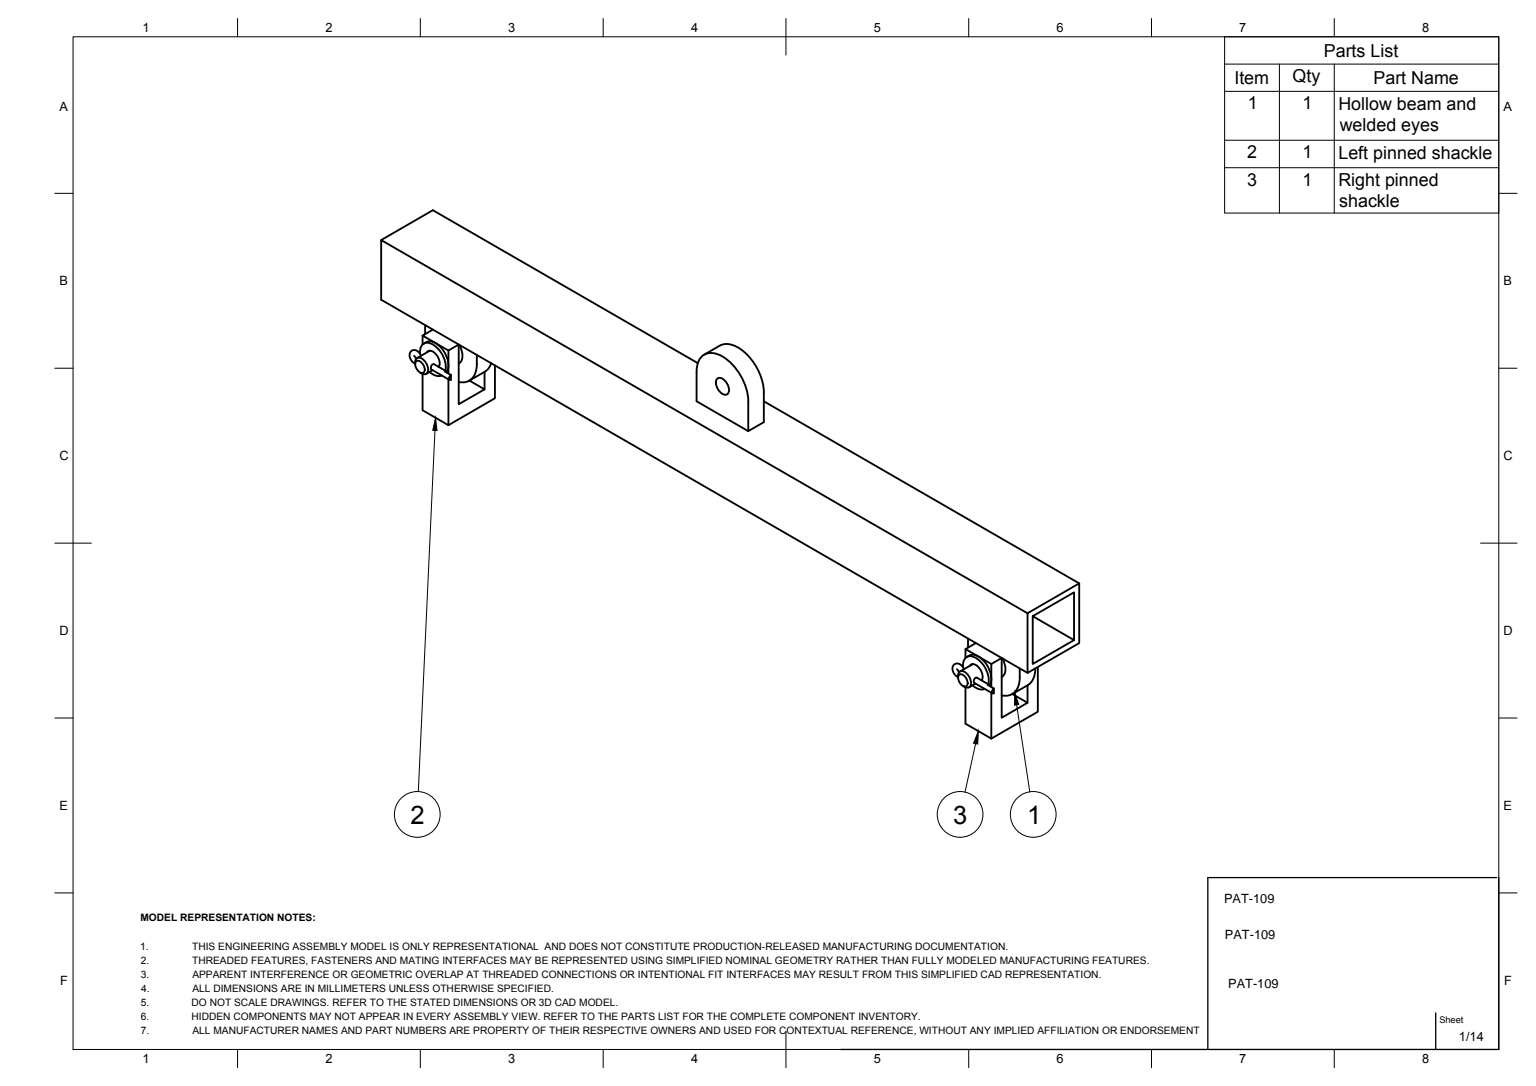
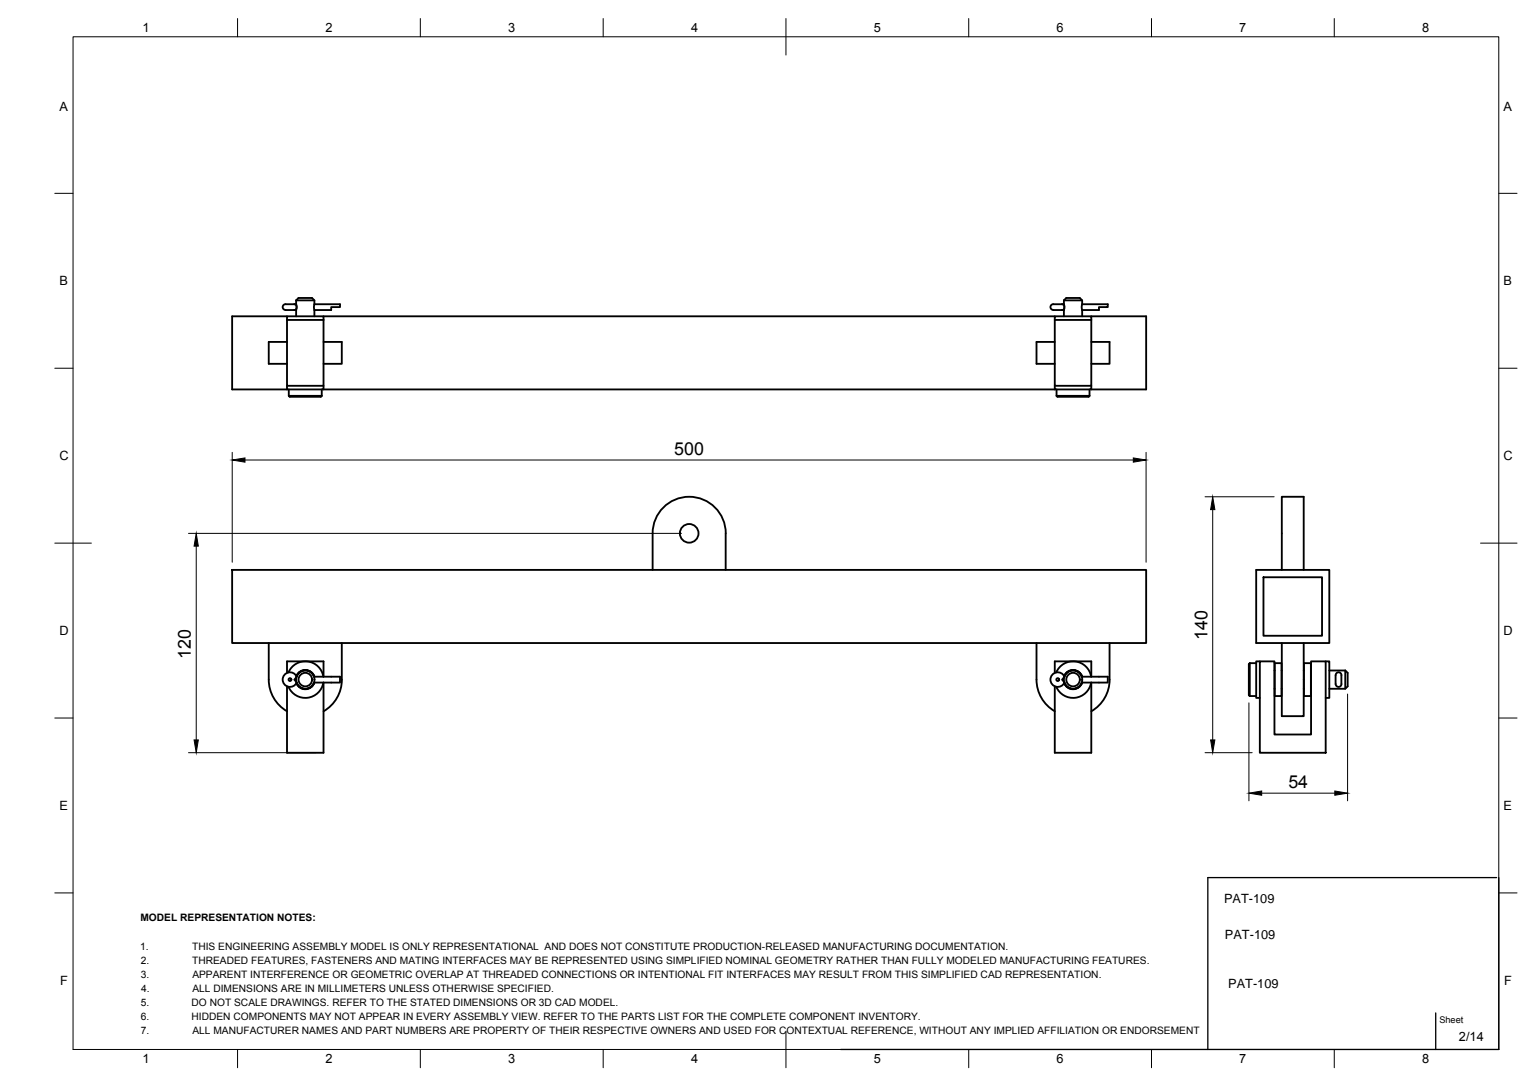
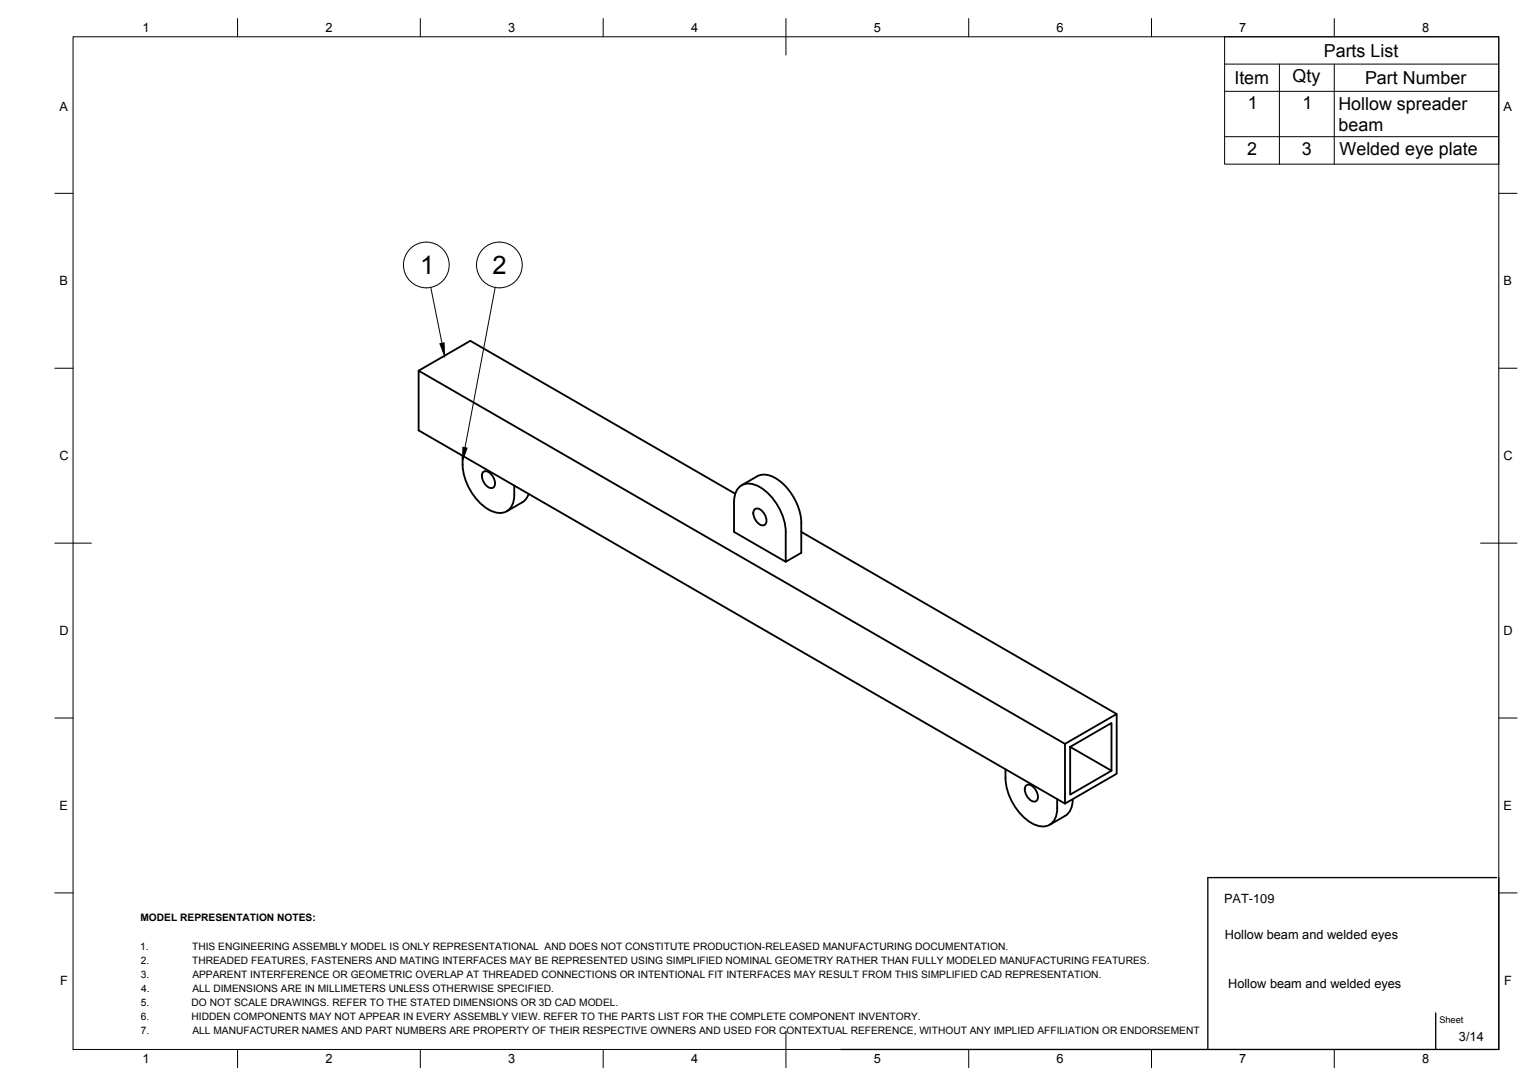
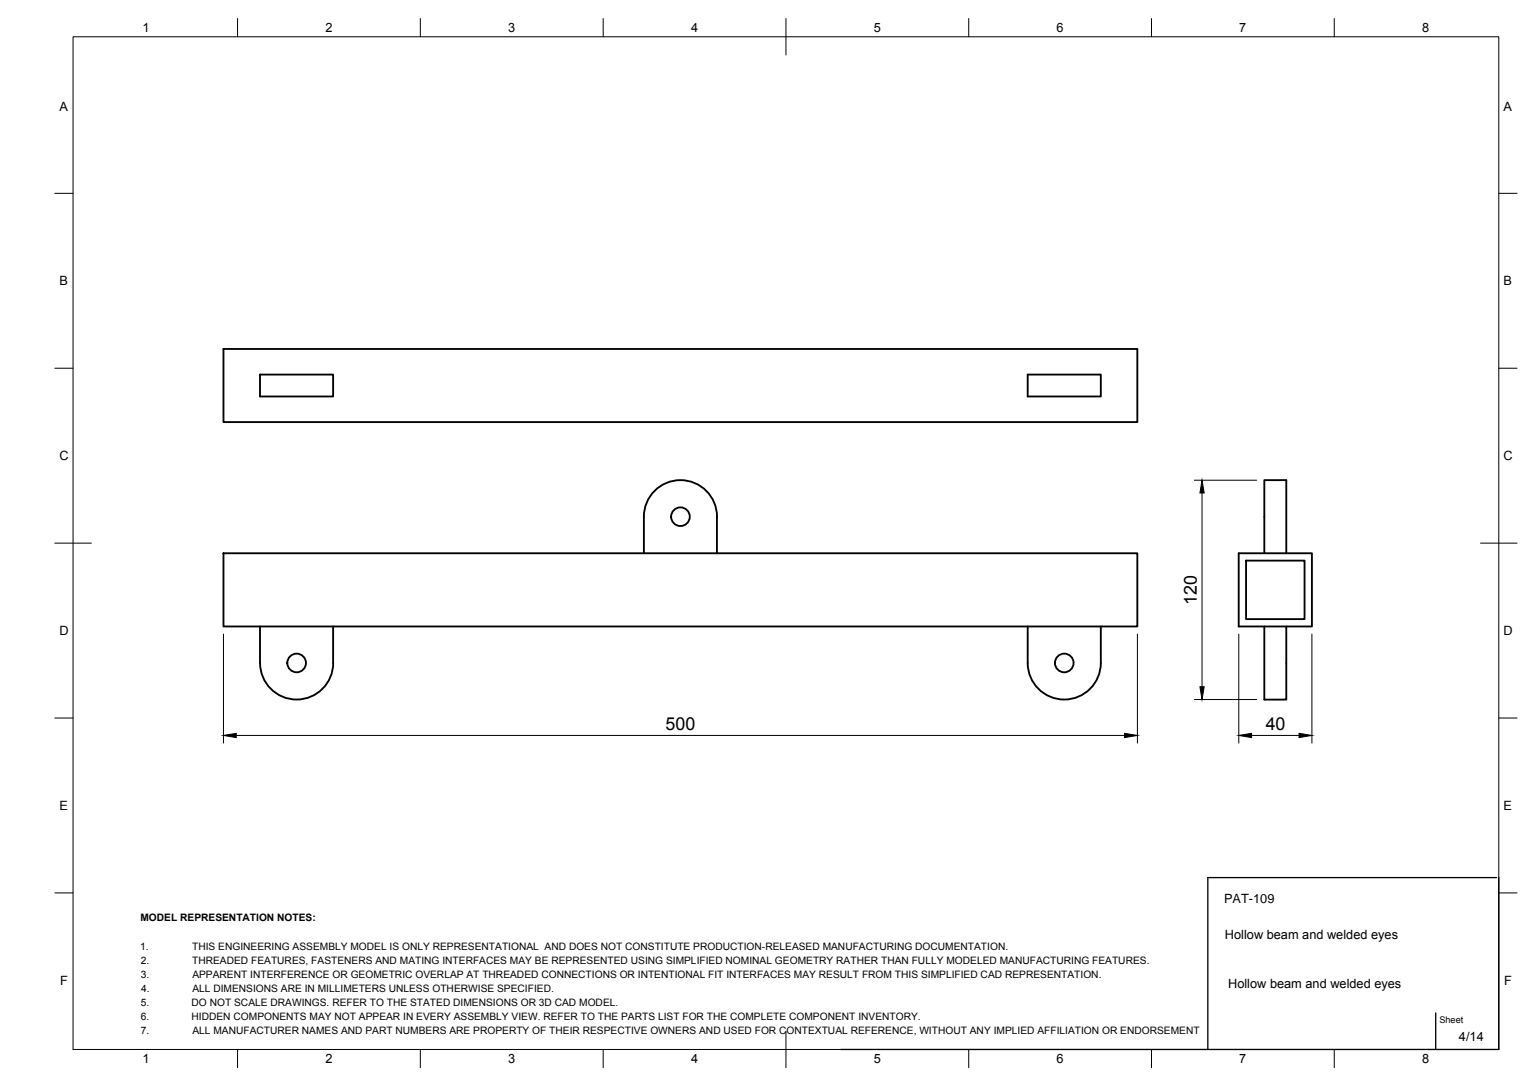
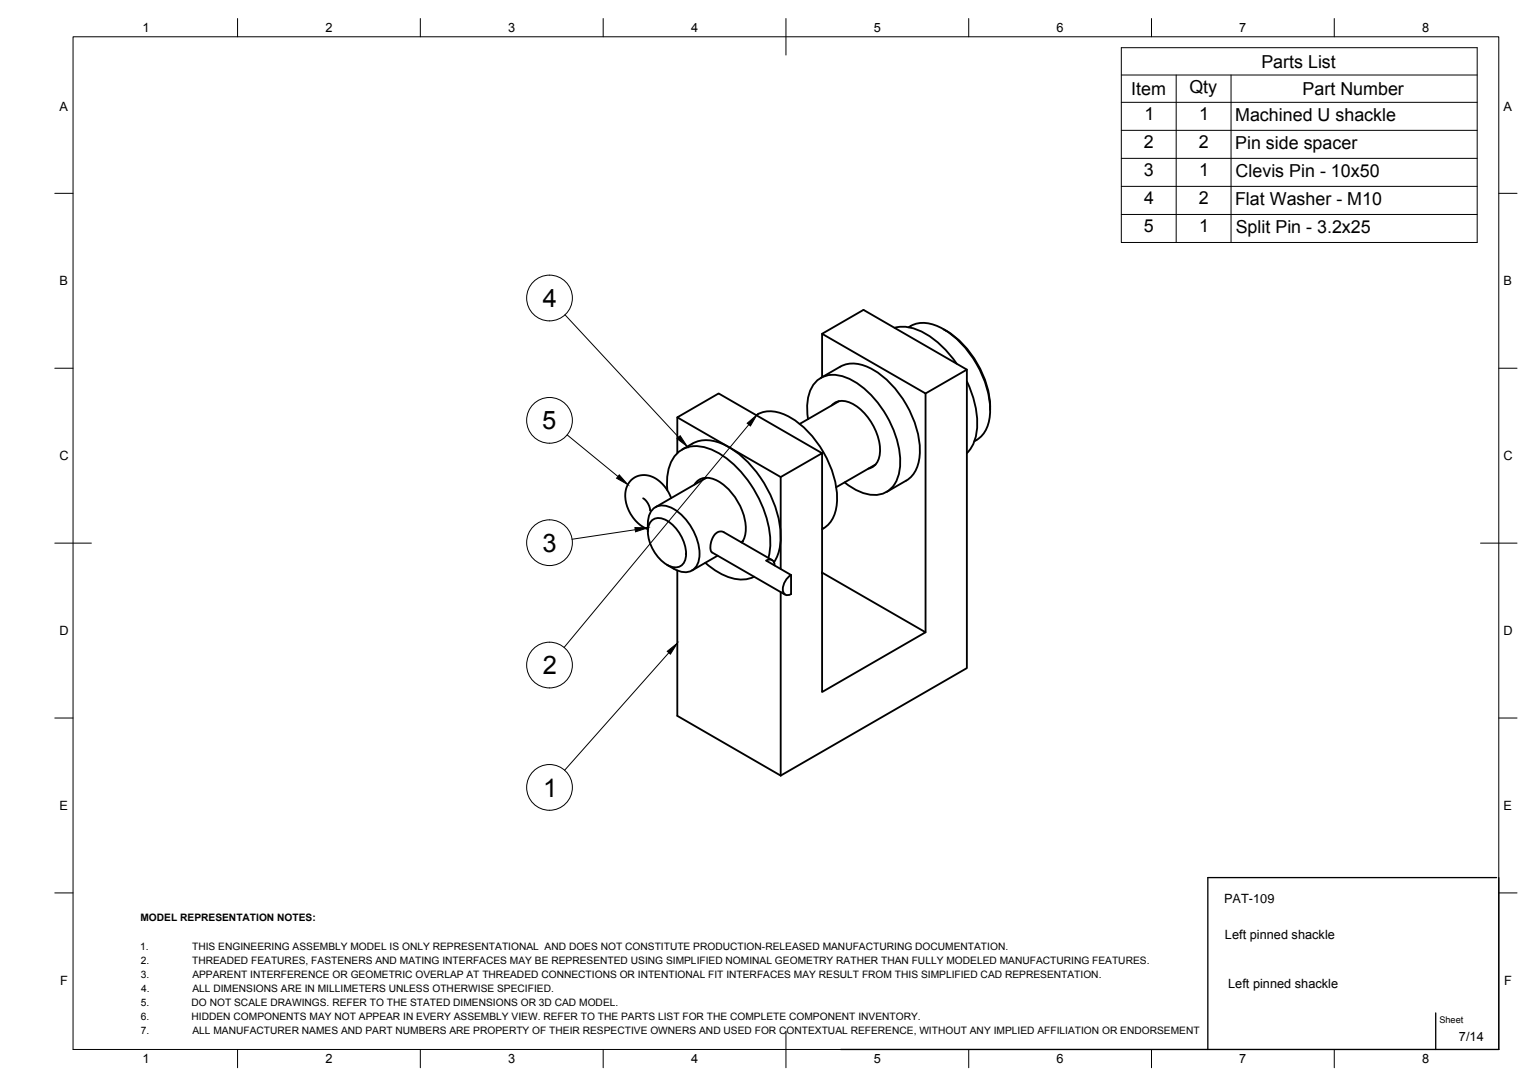
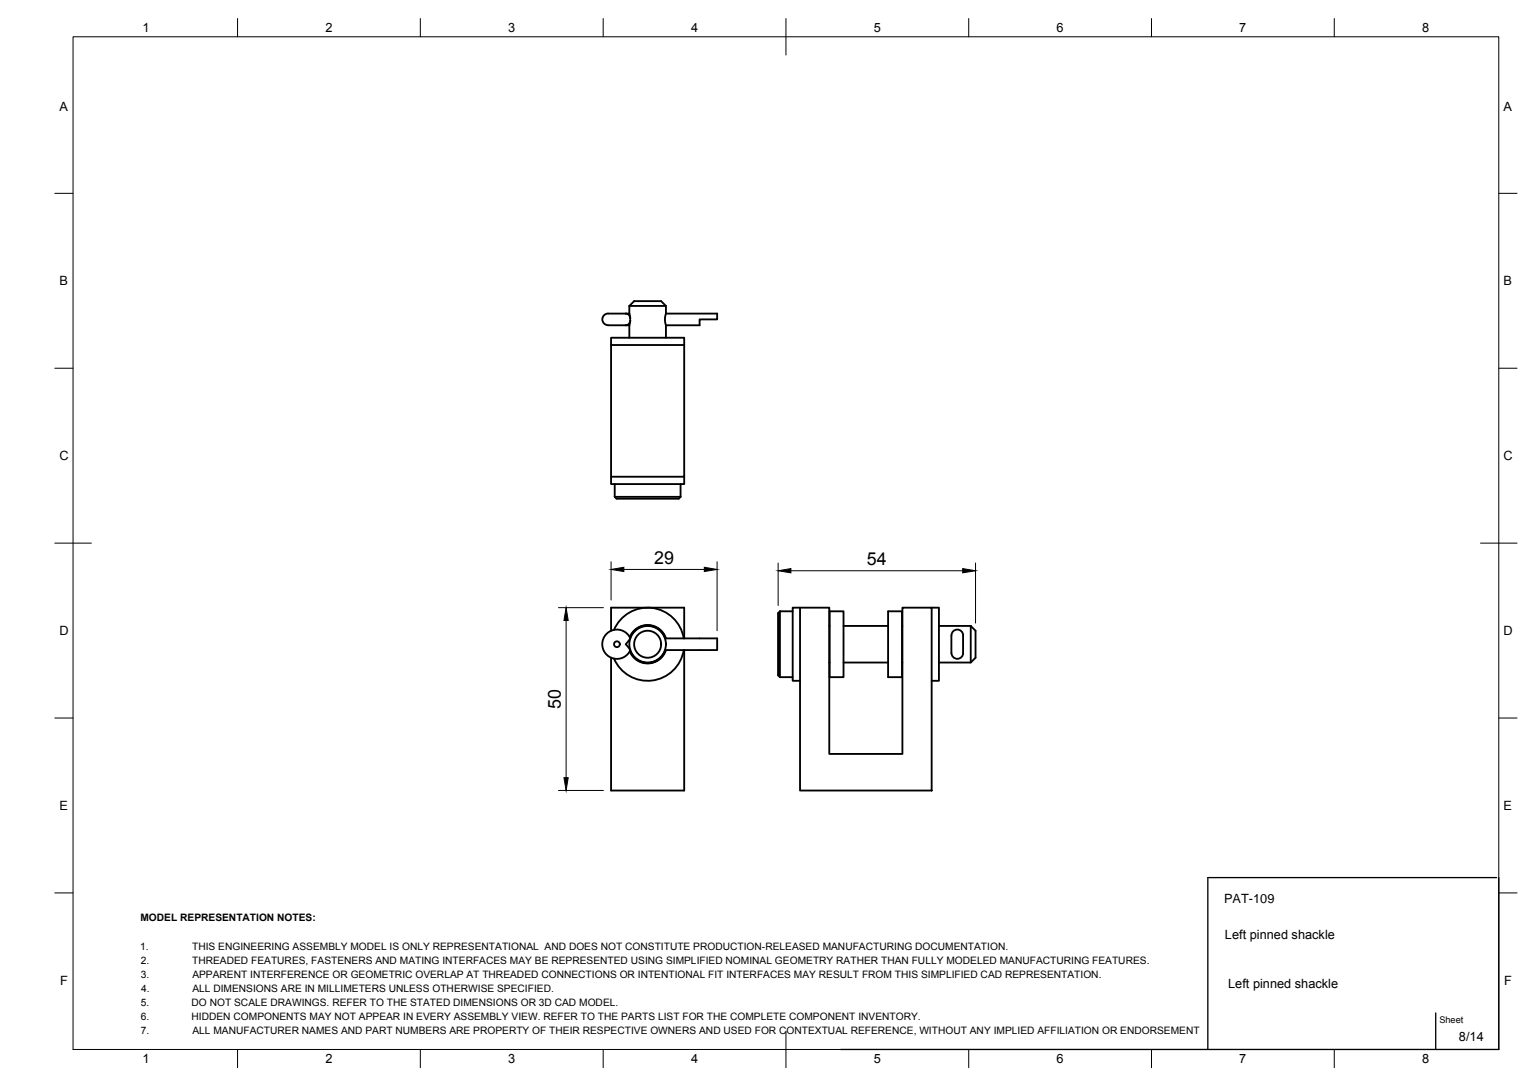
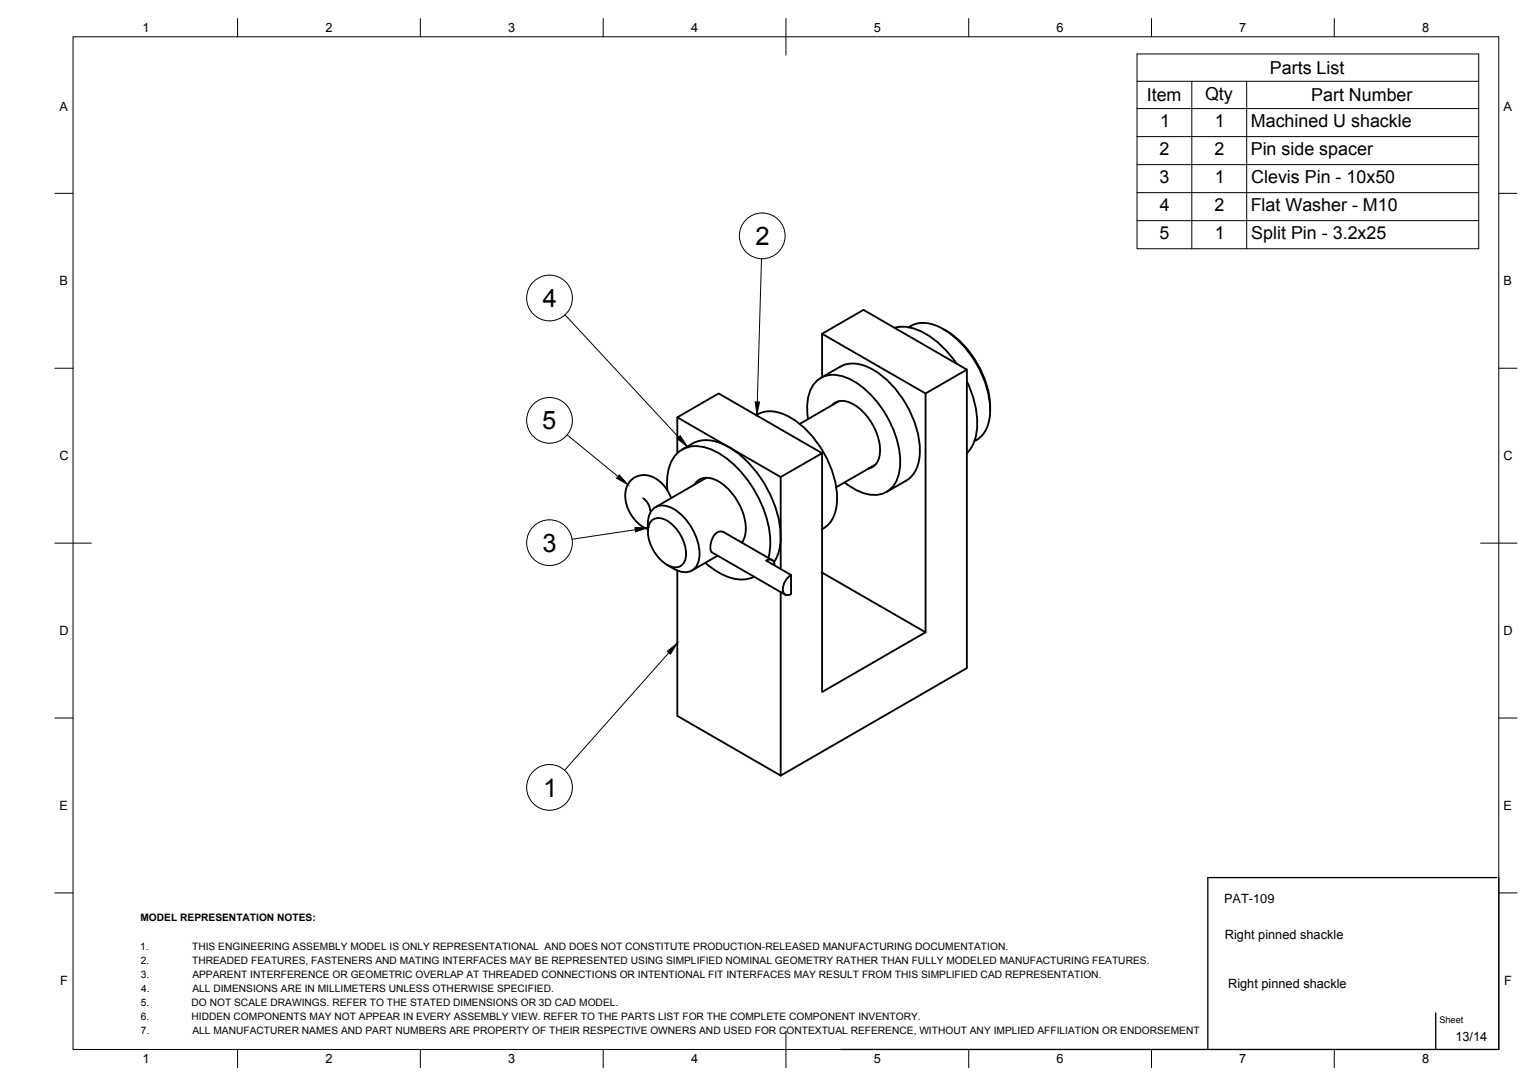
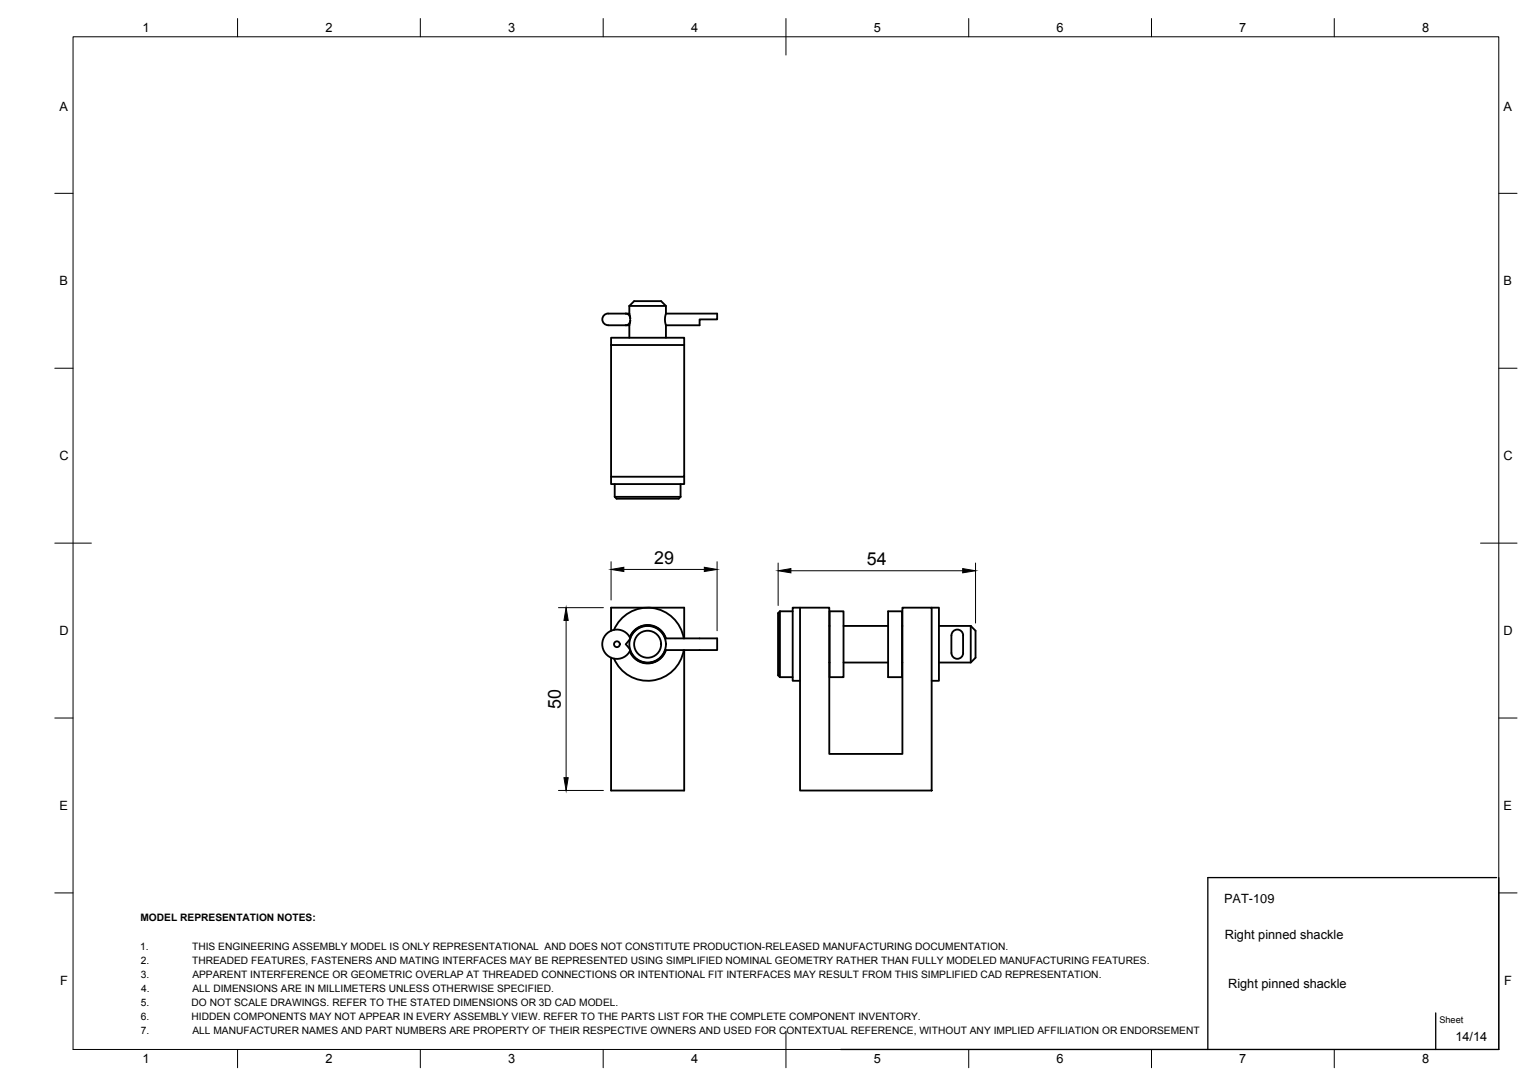
ISO-10303-21;
HEADER;
/* Generated by software containing ST-Developer
 * from STEP Tools, Inc. (www.steptools.com) 
 */

FILE_DESCRIPTION(
/* description */ ('Twin-shackle spreader bar'),
/* implementation_level */ '2;1');

FILE_NAME(
/* name */ 'PAT-109',
/* time_stamp */ '2026-10-27T20:18:10-07:00',
/* author */ (''),
/* organization */ (''),
/* preprocessor_version */ 'ST-DEVELOPER v20.2',
/* originating_system */ 'Autodesk Translation Framework v15.17.0.0',
/* authorisation */ '');

FILE_SCHEMA (('AUTOMOTIVE_DESIGN { 1 0 10303 214 3 1 1 }'));
ENDSEC;

DATA;
#10=MECHANICAL_DESIGN_GEOMETRIC_PRESENTATION_REPRESENTATION('',(#157,#158,
#159,#160,#161,#162,#163),#1829);
#11=TOROIDAL_SURFACE('',#1104,0.24,0.16);
#12=CONICAL_SURFACE('',#1083,0.875,0.785398163397448);
#13=CONICAL_SURFACE('',#1091,0.435,0.785398163397449);
#14=B_SPLINE_CURVE_WITH_KNOTS('',3,(#1599,#1600,#1601,#1602,#1603,#1604,
#1605,#1606,#1607,#1608),.UNSPECIFIED.,.F.,.F.,(4,2,2,2,4),(0.,0.0607460470679908,
0.121492094135982,0.182214421454286,0.242936748772591),.UNSPECIFIED.);
#15=B_SPLINE_CURVE_WITH_KNOTS('',3,(#1611,#1612,#1613,#1614,#1615,#1616,
#1617,#1618,#1619,#1620,#1621,#1622,#1623,#1624,#1625,#1626,#1627,#1628,
#1629,#1630,#1631,#1632,#1633,#1634,#1635,#1636,#1637,#1638,#1639,#1640,
#1641,#1642,#1643,#1644),.UNSPECIFIED.,.T.,.F.,(4,2,2,2,2,2,2,2,2,2,2,2,
2,2,2,2,4),(0.,0.0607460470679913,0.121492094135983,0.182214421454287,0.242936748772591,
0.303659076090896,0.3643814034092,0.425127450477191,0.485873497545182,0.546619544613173,
0.607365591681164,0.668087918999469,0.728810246317773,0.789532573636077,
0.850254900954382,0.911000948022373,0.971746995090363),.UNSPECIFIED.);
#16=B_SPLINE_CURVE_WITH_KNOTS('',3,(#1646,#1647,#1648,#1649,#1650,#1651,
#1652,#1653,#1654,#1655),.UNSPECIFIED.,.F.,.F.,(4,2,2,2,4),(0.728810246317772,
0.789532573636077,0.850254900954381,0.911000948022372,0.971746995090363),
 .UNSPECIFIED.);
#17=B_SPLINE_CURVE_WITH_KNOTS('',3,(#1656,#1657,#1658,#1659,#1660,#1661,
#1662,#1663,#1664,#1665,#1666,#1667,#1668,#1669,#1670,#1671,#1672,#1673),
 .UNSPECIFIED.,.F.,.F.,(4,2,2,2,2,2,2,2,4),(0.242936748772591,0.303659076090895,
0.364381403409199,0.42512745047719,0.485873497545182,0.546619544613173,
0.607365591681163,0.668087918999468,0.728810246317772),.UNSPECIFIED.);
#18=B_SPLINE_CURVE_WITH_KNOTS('',3,(#1720,#1721,#1722,#1723,#1724,#1725,
#1726,#1727,#1728,#1729,#1730,#1731,#1732,#1733,#1734,#1735,#1736,#1737,
#1738,#1739,#1740,#1741,#1742,#1743,#1744,#1745),.UNSPECIFIED.,.F.,.F.,
(4,2,2,2,2,2,2,2,2,2,2,2,4),(-0.000771405883143509,0.,0.0566386712389912,
0.124022719697233,0.181497823731714,0.241714216509916,0.290259365558526,
0.338804514607135,0.399020907385337,0.456496011419817,0.52388005987806,
0.580518731117043,0.581290137000192),.UNSPECIFIED.);
#19=B_SPLINE_CURVE_WITH_KNOTS('',3,(#1746,#1747,#1748,#1749,#1750,#1751,
#1752,#1753,#1754,#1755,#1756,#1757,#1758,#1759,#1760,#1761,#1762,#1763,
#1764,#1765,#1766,#1767,#1768,#1769,#1770,#1771),.UNSPECIFIED.,.F.,.F.,
(4,2,2,2,2,2,2,2,2,2,2,2,4),(-0.000771405883162359,0.,0.0566386712397236,
0.124022719698972,0.181497823734311,0.241714216513412,0.290259365562747,
0.338804514612082,0.399020907391184,0.456496011426523,0.523880059885771,
0.580518731125564,0.58129013700872),.UNSPECIFIED.);
#20=ITEM_DEFINED_TRANSFORMATION($,$,#1024,#1047);
#21=ITEM_DEFINED_TRANSFORMATION($,$,#1035,#1048);
#22=ITEM_DEFINED_TRANSFORMATION($,$,#1035,#1049);
#23=ITEM_DEFINED_TRANSFORMATION($,$,#1035,#1050);
#24=ITEM_DEFINED_TRANSFORMATION($,$,#1053,#1114);
#25=ITEM_DEFINED_TRANSFORMATION($,$,#1070,#1115);
#26=ITEM_DEFINED_TRANSFORMATION($,$,#1070,#1116);
#27=ITEM_DEFINED_TRANSFORMATION($,$,#1079,#1117);
#28=ITEM_DEFINED_TRANSFORMATION($,$,#1094,#1118);
#29=ITEM_DEFINED_TRANSFORMATION($,$,#1094,#1119);
#30=ITEM_DEFINED_TRANSFORMATION($,$,#1103,#1120);
#31=ITEM_DEFINED_TRANSFORMATION($,$,#1053,#1121);
#32=ITEM_DEFINED_TRANSFORMATION($,$,#1070,#1122);
#33=ITEM_DEFINED_TRANSFORMATION($,$,#1070,#1123);
#34=ITEM_DEFINED_TRANSFORMATION($,$,#1079,#1124);
#35=ITEM_DEFINED_TRANSFORMATION($,$,#1094,#1125);
#36=ITEM_DEFINED_TRANSFORMATION($,$,#1094,#1126);
#37=ITEM_DEFINED_TRANSFORMATION($,$,#1103,#1127);
#38=ITEM_DEFINED_TRANSFORMATION($,$,#1023,#1128);
#39=ITEM_DEFINED_TRANSFORMATION($,$,#1051,#1129);
#40=ITEM_DEFINED_TRANSFORMATION($,$,#1052,#1130);
#41=(
REPRESENTATION_RELATIONSHIP($,$,#1879,#1878)
REPRESENTATION_RELATIONSHIP_WITH_TRANSFORMATION(#20)
SHAPE_REPRESENTATION_RELATIONSHIP()
);
#42=(
REPRESENTATION_RELATIONSHIP($,$,#1880,#1878)
REPRESENTATION_RELATIONSHIP_WITH_TRANSFORMATION(#21)
SHAPE_REPRESENTATION_RELATIONSHIP()
);
#43=(
REPRESENTATION_RELATIONSHIP($,$,#1880,#1878)
REPRESENTATION_RELATIONSHIP_WITH_TRANSFORMATION(#22)
SHAPE_REPRESENTATION_RELATIONSHIP()
);
#44=(
REPRESENTATION_RELATIONSHIP($,$,#1880,#1878)
REPRESENTATION_RELATIONSHIP_WITH_TRANSFORMATION(#23)
SHAPE_REPRESENTATION_RELATIONSHIP()
);
#45=(
REPRESENTATION_RELATIONSHIP($,$,#1883,#1881)
REPRESENTATION_RELATIONSHIP_WITH_TRANSFORMATION(#24)
SHAPE_REPRESENTATION_RELATIONSHIP()
);
#46=(
REPRESENTATION_RELATIONSHIP($,$,#1884,#1881)
REPRESENTATION_RELATIONSHIP_WITH_TRANSFORMATION(#25)
SHAPE_REPRESENTATION_RELATIONSHIP()
);
#47=(
REPRESENTATION_RELATIONSHIP($,$,#1884,#1881)
REPRESENTATION_RELATIONSHIP_WITH_TRANSFORMATION(#26)
SHAPE_REPRESENTATION_RELATIONSHIP()
);
#48=(
REPRESENTATION_RELATIONSHIP($,$,#1885,#1881)
REPRESENTATION_RELATIONSHIP_WITH_TRANSFORMATION(#27)
SHAPE_REPRESENTATION_RELATIONSHIP()
);
#49=(
REPRESENTATION_RELATIONSHIP($,$,#1886,#1881)
REPRESENTATION_RELATIONSHIP_WITH_TRANSFORMATION(#28)
SHAPE_REPRESENTATION_RELATIONSHIP()
);
#50=(
REPRESENTATION_RELATIONSHIP($,$,#1886,#1881)
REPRESENTATION_RELATIONSHIP_WITH_TRANSFORMATION(#29)
SHAPE_REPRESENTATION_RELATIONSHIP()
);
#51=(
REPRESENTATION_RELATIONSHIP($,$,#1887,#1881)
REPRESENTATION_RELATIONSHIP_WITH_TRANSFORMATION(#30)
SHAPE_REPRESENTATION_RELATIONSHIP()
);
#52=(
REPRESENTATION_RELATIONSHIP($,$,#1883,#1882)
REPRESENTATION_RELATIONSHIP_WITH_TRANSFORMATION(#31)
SHAPE_REPRESENTATION_RELATIONSHIP()
);
#53=(
REPRESENTATION_RELATIONSHIP($,$,#1884,#1882)
REPRESENTATION_RELATIONSHIP_WITH_TRANSFORMATION(#32)
SHAPE_REPRESENTATION_RELATIONSHIP()
);
#54=(
REPRESENTATION_RELATIONSHIP($,$,#1884,#1882)
REPRESENTATION_RELATIONSHIP_WITH_TRANSFORMATION(#33)
SHAPE_REPRESENTATION_RELATIONSHIP()
);
#55=(
REPRESENTATION_RELATIONSHIP($,$,#1885,#1882)
REPRESENTATION_RELATIONSHIP_WITH_TRANSFORMATION(#34)
SHAPE_REPRESENTATION_RELATIONSHIP()
);
#56=(
REPRESENTATION_RELATIONSHIP($,$,#1886,#1882)
REPRESENTATION_RELATIONSHIP_WITH_TRANSFORMATION(#35)
SHAPE_REPRESENTATION_RELATIONSHIP()
);
#57=(
REPRESENTATION_RELATIONSHIP($,$,#1886,#1882)
REPRESENTATION_RELATIONSHIP_WITH_TRANSFORMATION(#36)
SHAPE_REPRESENTATION_RELATIONSHIP()
);
#58=(
REPRESENTATION_RELATIONSHIP($,$,#1887,#1882)
REPRESENTATION_RELATIONSHIP_WITH_TRANSFORMATION(#37)
SHAPE_REPRESENTATION_RELATIONSHIP()
);
#59=(
REPRESENTATION_RELATIONSHIP($,$,#1878,#1877)
REPRESENTATION_RELATIONSHIP_WITH_TRANSFORMATION(#38)
SHAPE_REPRESENTATION_RELATIONSHIP()
);
#60=(
REPRESENTATION_RELATIONSHIP($,$,#1881,#1877)
REPRESENTATION_RELATIONSHIP_WITH_TRANSFORMATION(#39)
SHAPE_REPRESENTATION_RELATIONSHIP()
);
#61=(
REPRESENTATION_RELATIONSHIP($,$,#1882,#1877)
REPRESENTATION_RELATIONSHIP_WITH_TRANSFORMATION(#40)
SHAPE_REPRESENTATION_RELATIONSHIP()
);
#62=CONTEXT_DEPENDENT_SHAPE_REPRESENTATION(#41,#1849);
#63=CONTEXT_DEPENDENT_SHAPE_REPRESENTATION(#42,#1850);
#64=CONTEXT_DEPENDENT_SHAPE_REPRESENTATION(#43,#1851);
#65=CONTEXT_DEPENDENT_SHAPE_REPRESENTATION(#44,#1852);
#66=CONTEXT_DEPENDENT_SHAPE_REPRESENTATION(#45,#1860);
#67=CONTEXT_DEPENDENT_SHAPE_REPRESENTATION(#46,#1861);
#68=CONTEXT_DEPENDENT_SHAPE_REPRESENTATION(#47,#1862);
#69=CONTEXT_DEPENDENT_SHAPE_REPRESENTATION(#48,#1863);
#70=CONTEXT_DEPENDENT_SHAPE_REPRESENTATION(#49,#1864);
#71=CONTEXT_DEPENDENT_SHAPE_REPRESENTATION(#50,#1865);
#72=CONTEXT_DEPENDENT_SHAPE_REPRESENTATION(#51,#1866);
#73=CONTEXT_DEPENDENT_SHAPE_REPRESENTATION(#52,#1867);
#74=CONTEXT_DEPENDENT_SHAPE_REPRESENTATION(#53,#1868);
#75=CONTEXT_DEPENDENT_SHAPE_REPRESENTATION(#54,#1869);
#76=CONTEXT_DEPENDENT_SHAPE_REPRESENTATION(#55,#1870);
#77=CONTEXT_DEPENDENT_SHAPE_REPRESENTATION(#56,#1871);
#78=CONTEXT_DEPENDENT_SHAPE_REPRESENTATION(#57,#1872);
#79=CONTEXT_DEPENDENT_SHAPE_REPRESENTATION(#58,#1873);
#80=CONTEXT_DEPENDENT_SHAPE_REPRESENTATION(#59,#1874);
#81=CONTEXT_DEPENDENT_SHAPE_REPRESENTATION(#60,#1875);
#82=CONTEXT_DEPENDENT_SHAPE_REPRESENTATION(#61,#1876);
#83=NEXT_ASSEMBLY_USAGE_OCCURRENCE('Hollow spreader beam:1',
'Hollow spreader beam:1','Hollow spreader beam:1',#1890,#1891,
'Hollow spreader beam:1');
#84=NEXT_ASSEMBLY_USAGE_OCCURRENCE('Welded eye plate:1',
'Welded eye plate:1','Welded eye plate:1',#1890,#1892,
'Welded eye plate:1');
#85=NEXT_ASSEMBLY_USAGE_OCCURRENCE('Welded eye plate:2',
'Welded eye plate:2','Welded eye plate:2',#1890,#1892,
'Welded eye plate:2');
#86=NEXT_ASSEMBLY_USAGE_OCCURRENCE('Welded eye plate:3',
'Welded eye plate:3','Welded eye plate:3',#1890,#1892,
'Welded eye plate:3');
#87=NEXT_ASSEMBLY_USAGE_OCCURRENCE('Machined U shackle:1',
'Machined U shackle:1','Machined U shackle:1',#1893,#1895,
'Machined U shackle:1');
#88=NEXT_ASSEMBLY_USAGE_OCCURRENCE('Pin side spacer:1',
'Pin side spacer:1','Pin side spacer:1',#1893,#1896,'Pin side spacer:1');
#89=NEXT_ASSEMBLY_USAGE_OCCURRENCE('Pin side spacer:2',
'Pin side spacer:2','Pin side spacer:2',#1893,#1896,'Pin side spacer:2');
#90=NEXT_ASSEMBLY_USAGE_OCCURRENCE('Clevis Pin - 10x50:2',
'Clevis Pin - 10x50:2','Clevis Pin - 10x50:2',#1893,#1897,
'Clevis Pin - 10x50:2');
#91=NEXT_ASSEMBLY_USAGE_OCCURRENCE('Flat Washer - M10:2',
'Flat Washer - M10:2','Flat Washer - M10:2',#1893,#1898,
'Flat Washer - M10:2');
#92=NEXT_ASSEMBLY_USAGE_OCCURRENCE('Flat Washer - M10:3',
'Flat Washer - M10:3','Flat Washer - M10:3',#1893,#1898,
'Flat Washer - M10:3');
#93=NEXT_ASSEMBLY_USAGE_OCCURRENCE('Split Pin - 3.2x25:2',
'Split Pin - 3.2x25:2','Split Pin - 3.2x25:2',#1893,#1899,
'Split Pin - 3.2x25:2');
#94=NEXT_ASSEMBLY_USAGE_OCCURRENCE('Machined U shackle:2',
'Machined U shackle:2','Machined U shackle:2',#1894,#1895,
'Machined U shackle:2');
#95=NEXT_ASSEMBLY_USAGE_OCCURRENCE('Pin side spacer:3',
'Pin side spacer:3','Pin side spacer:3',#1894,#1896,'Pin side spacer:3');
#96=NEXT_ASSEMBLY_USAGE_OCCURRENCE('Pin side spacer:4',
'Pin side spacer:4','Pin side spacer:4',#1894,#1896,'Pin side spacer:4');
#97=NEXT_ASSEMBLY_USAGE_OCCURRENCE('Clevis Pin - 10x50:3',
'Clevis Pin - 10x50:3','Clevis Pin - 10x50:3',#1894,#1897,
'Clevis Pin - 10x50:3');
#98=NEXT_ASSEMBLY_USAGE_OCCURRENCE('Flat Washer - M10:4',
'Flat Washer - M10:4','Flat Washer - M10:4',#1894,#1898,
'Flat Washer - M10:4');
#99=NEXT_ASSEMBLY_USAGE_OCCURRENCE('Flat Washer - M10:5',
'Flat Washer - M10:5','Flat Washer - M10:5',#1894,#1898,
'Flat Washer - M10:5');
#100=NEXT_ASSEMBLY_USAGE_OCCURRENCE('Split Pin - 3.2x25:3',
'Split Pin - 3.2x25:3','Split Pin - 3.2x25:3',#1894,#1899,
'Split Pin - 3.2x25:3');
#101=NEXT_ASSEMBLY_USAGE_OCCURRENCE('Hollow beam and welded eyes:1',
'Hollow beam and welded eyes:1','Hollow beam and welded eyes:1',#1889,#1890,
'Hollow beam and welded eyes:1');
#102=NEXT_ASSEMBLY_USAGE_OCCURRENCE('Left pinned shackle:1',
'Left pinned shackle:1','Left pinned shackle:1',#1889,#1893,
'Left pinned shackle:1');
#103=NEXT_ASSEMBLY_USAGE_OCCURRENCE('Right pinned shackle:1',
'Right pinned shackle:1','Right pinned shackle:1',#1889,#1894,
'Right pinned shackle:1');
#104=CIRCLE('',#1037,0.510000000000002);
#105=CIRCLE('',#1038,0.510000000000002);
#106=CIRCLE('',#1043,2.);
#107=CIRCLE('',#1045,2.);
#108=CIRCLE('',#1055,0.515000000000001);
#109=CIRCLE('',#1056,0.515000000000001);
#110=CIRCLE('',#1058,0.515000000000001);
#111=CIRCLE('',#1059,0.515000000000001);
#112=CIRCLE('',#1072,0.510000000000002);
#113=CIRCLE('',#1073,0.510000000000002);
#114=CIRCLE('',#1075,0.899999999999999);
#115=CIRCLE('',#1076,0.899999999999999);
#116=CIRCLE('',#1082,0.85);
#117=CIRCLE('',#1084,0.9);
#118=CIRCLE('',#1086,0.9);
#119=CIRCLE('',#1088,0.5);
#120=CIRCLE('',#1090,0.5);
#121=CIRCLE('',#1092,0.37);
#122=CIRCLE('',#1096,0.525);
#123=CIRCLE('',#1097,0.525);
#124=CIRCLE('',#1099,1.);
#125=CIRCLE('',#1100,1.);
#126=CIRCLE('',#1105,0.16);
#127=CIRCLE('',#1106,0.08);
#128=CIRCLE('',#1108,0.16);
#129=CIRCLE('',#1111,0.16);
#130=CIRCLE('',#1112,0.16);
#131=CYLINDRICAL_SURFACE('',#1036,0.510000000000002);
#132=CYLINDRICAL_SURFACE('',#1044,2.);
#133=CYLINDRICAL_SURFACE('',#1054,0.515000000000001);
#134=CYLINDRICAL_SURFACE('',#1057,0.515000000000001);
#135=CYLINDRICAL_SURFACE('',#1071,0.510000000000002);
#136=CYLINDRICAL_SURFACE('',#1074,0.899999999999999);
#137=CYLINDRICAL_SURFACE('',#1080,0.16);
#138=CYLINDRICAL_SURFACE('',#1085,0.9);
#139=CYLINDRICAL_SURFACE('',#1089,0.5);
#140=CYLINDRICAL_SURFACE('',#1095,0.525);
#141=CYLINDRICAL_SURFACE('',#1098,1.);
#142=CYLINDRICAL_SURFACE('',#1110,0.16);
#143=SHAPE_REPRESENTATION_RELATIONSHIP('SRR','None',#1879,#150);
#144=SHAPE_REPRESENTATION_RELATIONSHIP('SRR','None',#1880,#151);
#145=SHAPE_REPRESENTATION_RELATIONSHIP('SRR','None',#1883,#152);
#146=SHAPE_REPRESENTATION_RELATIONSHIP('SRR','None',#1884,#153);
#147=SHAPE_REPRESENTATION_RELATIONSHIP('SRR','None',#1885,#154);
#148=SHAPE_REPRESENTATION_RELATIONSHIP('SRR','None',#1886,#155);
#149=SHAPE_REPRESENTATION_RELATIONSHIP('SRR','None',#1887,#156);
#150=ADVANCED_BREP_SHAPE_REPRESENTATION('',(#164),#1820);
#151=ADVANCED_BREP_SHAPE_REPRESENTATION('',(#165),#1821);
#152=ADVANCED_BREP_SHAPE_REPRESENTATION('',(#166),#1824);
#153=ADVANCED_BREP_SHAPE_REPRESENTATION('',(#167),#1825);
#154=ADVANCED_BREP_SHAPE_REPRESENTATION('',(#168),#1826);
#155=ADVANCED_BREP_SHAPE_REPRESENTATION('',(#169),#1827);
#156=ADVANCED_BREP_SHAPE_REPRESENTATION('',(#170),#1828);
#157=STYLED_ITEM('',(#1977),#164);
#158=STYLED_ITEM('',(#1977),#165);
#159=STYLED_ITEM('',(#1970),#166);
#160=STYLED_ITEM('',(#1984),#167);
#161=STYLED_ITEM('',(#1984),#168);
#162=STYLED_ITEM('',(#1991),#169);
#163=STYLED_ITEM('',(#1984),#170);
#164=MANIFOLD_SOLID_BREP('Body1',#937);
#165=MANIFOLD_SOLID_BREP('Body1',#938);
#166=MANIFOLD_SOLID_BREP('Body1',#939);
#167=MANIFOLD_SOLID_BREP('Body1',#940);
#168=MANIFOLD_SOLID_BREP('Body1',#941);
#169=MANIFOLD_SOLID_BREP('Body1',#942);
#170=MANIFOLD_SOLID_BREP('Body1',#943);
#171=FACE_BOUND('',#242,.T.);
#172=FACE_BOUND('',#245,.T.);
#173=FACE_BOUND('',#253,.T.);
#174=FACE_BOUND('',#256,.T.);
#175=FACE_BOUND('',#260,.T.);
#176=FACE_BOUND('',#263,.T.);
#177=FACE_BOUND('',#266,.T.);
#178=FACE_BOUND('',#269,.T.);
#179=FACE_BOUND('',#276,.T.);
#180=FACE_BOUND('',#278,.T.);
#181=FACE_BOUND('',#284,.T.);
#182=FACE_BOUND('',#286,.T.);
#183=FACE_BOUND('',#292,.T.);
#184=FACE_BOUND('',#294,.T.);
#185=FACE_BOUND('',#296,.T.);
#186=FACE_OUTER_BOUND('',#236,.T.);
#187=FACE_OUTER_BOUND('',#237,.T.);
#188=FACE_OUTER_BOUND('',#238,.T.);
#189=FACE_OUTER_BOUND('',#239,.T.);
#190=FACE_OUTER_BOUND('',#240,.T.);
#191=FACE_OUTER_BOUND('',#241,.T.);
#192=FACE_OUTER_BOUND('',#243,.T.);
#193=FACE_OUTER_BOUND('',#244,.T.);
#194=FACE_OUTER_BOUND('',#246,.T.);
#195=FACE_OUTER_BOUND('',#247,.T.);
#196=FACE_OUTER_BOUND('',#248,.T.);
#197=FACE_OUTER_BOUND('',#249,.T.);
#198=FACE_OUTER_BOUND('',#250,.T.);
#199=FACE_OUTER_BOUND('',#251,.T.);
#200=FACE_OUTER_BOUND('',#252,.T.);
#201=FACE_OUTER_BOUND('',#254,.T.);
#202=FACE_OUTER_BOUND('',#255,.T.);
#203=FACE_OUTER_BOUND('',#257,.T.);
#204=FACE_OUTER_BOUND('',#258,.T.);
#205=FACE_OUTER_BOUND('',#259,.T.);
#206=FACE_OUTER_BOUND('',#261,.T.);
#207=FACE_OUTER_BOUND('',#262,.T.);
#208=FACE_OUTER_BOUND('',#264,.T.);
#209=FACE_OUTER_BOUND('',#265,.T.);
#210=FACE_OUTER_BOUND('',#267,.T.);
#211=FACE_OUTER_BOUND('',#268,.T.);
#212=FACE_OUTER_BOUND('',#270,.T.);
#213=FACE_OUTER_BOUND('',#271,.T.);
#214=FACE_OUTER_BOUND('',#272,.T.);
#215=FACE_OUTER_BOUND('',#273,.T.);
#216=FACE_OUTER_BOUND('',#274,.T.);
#217=FACE_OUTER_BOUND('',#275,.T.);
#218=FACE_OUTER_BOUND('',#277,.T.);
#219=FACE_OUTER_BOUND('',#279,.T.);
#220=FACE_OUTER_BOUND('',#280,.T.);
#221=FACE_OUTER_BOUND('',#281,.T.);
#222=FACE_OUTER_BOUND('',#282,.T.);
#223=FACE_OUTER_BOUND('',#283,.T.);
#224=FACE_OUTER_BOUND('',#285,.T.);
#225=FACE_OUTER_BOUND('',#287,.T.);
#226=FACE_OUTER_BOUND('',#288,.T.);
#227=FACE_OUTER_BOUND('',#289,.T.);
#228=FACE_OUTER_BOUND('',#290,.T.);
#229=FACE_OUTER_BOUND('',#291,.T.);
#230=FACE_OUTER_BOUND('',#293,.T.);
#231=FACE_OUTER_BOUND('',#295,.T.);
#232=FACE_OUTER_BOUND('',#297,.T.);
#233=FACE_OUTER_BOUND('',#298,.T.);
#234=FACE_OUTER_BOUND('',#299,.T.);
#235=FACE_OUTER_BOUND('',#300,.T.);
#236=EDGE_LOOP('',(#634,#635,#636,#637));
#237=EDGE_LOOP('',(#638,#639,#640,#641));
#238=EDGE_LOOP('',(#642,#643,#644,#645));
#239=EDGE_LOOP('',(#646,#647,#648,#649));
#240=EDGE_LOOP('',(#650,#651,#652,#653));
#241=EDGE_LOOP('',(#654,#655,#656,#657));
#242=EDGE_LOOP('',(#658,#659,#660,#661));
#243=EDGE_LOOP('',(#662,#663,#664,#665));
#244=EDGE_LOOP('',(#666,#667,#668,#669));
#245=EDGE_LOOP('',(#670,#671,#672,#673));
#246=EDGE_LOOP('',(#674,#675,#676,#677));
#247=EDGE_LOOP('',(#678,#679,#680,#681));
#248=EDGE_LOOP('',(#682,#683,#684,#685));
#249=EDGE_LOOP('',(#686,#687,#688,#689));
#250=EDGE_LOOP('',(#690,#691,#692,#693));
#251=EDGE_LOOP('',(#694,#695,#696,#697));
#252=EDGE_LOOP('',(#698,#699,#700,#701));
#253=EDGE_LOOP('',(#702));
#254=EDGE_LOOP('',(#703,#704,#705,#706));
#255=EDGE_LOOP('',(#707,#708,#709,#710));
#256=EDGE_LOOP('',(#711));
#257=EDGE_LOOP('',(#712,#713,#714,#715));
#258=EDGE_LOOP('',(#716,#717,#718,#719));
#259=EDGE_LOOP('',(#720,#721,#722,#723));
#260=EDGE_LOOP('',(#724));
#261=EDGE_LOOP('',(#725,#726,#727,#728));
#262=EDGE_LOOP('',(#729,#730,#731,#732));
#263=EDGE_LOOP('',(#733));
#264=EDGE_LOOP('',(#734,#735,#736,#737));
#265=EDGE_LOOP('',(#738,#739,#740,#741));
#266=EDGE_LOOP('',(#742));
#267=EDGE_LOOP('',(#743,#744,#745,#746));
#268=EDGE_LOOP('',(#747,#748,#749,#750));
#269=EDGE_LOOP('',(#751));
#270=EDGE_LOOP('',(#752,#753,#754,#755));
#271=EDGE_LOOP('',(#756,#757,#758,#759,#760,#761,#762,#763));
#272=EDGE_LOOP('',(#764,#765,#766,#767,#768,#769,#770,#771));
#273=EDGE_LOOP('',(#772,#773,#774,#775));
#274=EDGE_LOOP('',(#776,#777,#778,#779));
#275=EDGE_LOOP('',(#780));
#276=EDGE_LOOP('',(#781));
#277=EDGE_LOOP('',(#782));
#278=EDGE_LOOP('',(#783));
#279=EDGE_LOOP('',(#784,#785,#786,#787,#788,#789));
#280=EDGE_LOOP('',(#790));
#281=EDGE_LOOP('',(#791,#792,#793,#794));
#282=EDGE_LOOP('',(#795,#796,#797,#798));
#283=EDGE_LOOP('',(#799));
#284=EDGE_LOOP('',(#800));
#285=EDGE_LOOP('',(#801,#802,#803,#804,#805,#806,#807,#808,#809));
#286=EDGE_LOOP('',(#810));
#287=EDGE_LOOP('',(#811,#812,#813,#814));
#288=EDGE_LOOP('',(#815));
#289=EDGE_LOOP('',(#816,#817,#818,#819));
#290=EDGE_LOOP('',(#820,#821,#822,#823));
#291=EDGE_LOOP('',(#824));
#292=EDGE_LOOP('',(#825));
#293=EDGE_LOOP('',(#826));
#294=EDGE_LOOP('',(#827));
#295=EDGE_LOOP('',(#828,#829,#830,#831));
#296=EDGE_LOOP('',(#832,#833));
#297=EDGE_LOOP('',(#834,#835));
#298=EDGE_LOOP('',(#836,#837,#838,#839));
#299=EDGE_LOOP('',(#840,#841,#842,#843,#844,#845,#846,#847,#848));
#300=EDGE_LOOP('',(#849,#850,#851));
#301=LINE('',#1431,#377);
#302=LINE('',#1433,#378);
#303=LINE('',#1435,#379);
#304=LINE('',#1436,#380);
#305=LINE('',#1439,#381);
#306=LINE('',#1441,#382);
#307=LINE('',#1442,#383);
#308=LINE('',#1445,#384);
#309=LINE('',#1447,#385);
#310=LINE('',#1448,#386);
#311=LINE('',#1450,#387);
#312=LINE('',#1451,#388);
#313=LINE('',#1455,#389);
#314=LINE('',#1457,#390);
#315=LINE('',#1459,#391);
#316=LINE('',#1460,#392);
#317=LINE('',#1463,#393);
#318=LINE('',#1465,#394);
#319=LINE('',#1466,#395);
#320=LINE('',#1469,#396);
#321=LINE('',#1471,#397);
#322=LINE('',#1472,#398);
#323=LINE('',#1474,#399);
#324=LINE('',#1475,#400);
#325=LINE('',#1483,#401);
#326=LINE('',#1488,#402);
#327=LINE('',#1490,#403);
#328=LINE('',#1492,#404);
#329=LINE('',#1493,#405);
#330=LINE('',#1497,#406);
#331=LINE('',#1499,#407);
#332=LINE('',#1501,#408);
#333=LINE('',#1502,#409);
#334=LINE('',#1504,#410);
#335=LINE('',#1505,#411);
#336=LINE('',#1522,#412);
#337=LINE('',#1528,#413);
#338=LINE('',#1533,#414);
#339=LINE('',#1535,#415);
#340=LINE('',#1537,#416);
#341=LINE('',#1538,#417);
#342=LINE('',#1541,#418);
#343=LINE('',#1543,#419);
#344=LINE('',#1544,#420);
#345=LINE('',#1547,#421);
#346=LINE('',#1549,#422);
#347=LINE('',#1550,#423);
#348=LINE('',#1553,#424);
#349=LINE('',#1555,#425);
#350=LINE('',#1556,#426);
#351=LINE('',#1559,#427);
#352=LINE('',#1561,#428);
#353=LINE('',#1562,#429);
#354=LINE('',#1565,#430);
#355=LINE('',#1567,#431);
#356=LINE('',#1568,#432);
#357=LINE('',#1571,#433);
#358=LINE('',#1573,#434);
#359=LINE('',#1574,#435);
#360=LINE('',#1576,#436);
#361=LINE('',#1577,#437);
#362=LINE('',#1585,#438);
#363=LINE('',#1591,#439);
#364=LINE('',#1610,#440);
#365=LINE('',#1680,#441);
#366=LINE('',#1684,#442);
#367=LINE('',#1691,#443);
#368=LINE('',#1692,#444);
#369=LINE('',#1696,#445);
#370=LINE('',#1703,#446);
#371=LINE('',#1709,#447);
#372=LINE('',#1776,#448);
#373=LINE('',#1779,#449);
#374=LINE('',#1781,#450);
#375=LINE('',#1782,#451);
#376=LINE('',#1786,#452);
#377=VECTOR('',#1139,1.);
#378=VECTOR('',#1140,1.);
#379=VECTOR('',#1141,1.);
#380=VECTOR('',#1142,1.);
#381=VECTOR('',#1145,1.);
#382=VECTOR('',#1146,1.);
#383=VECTOR('',#1147,1.);
#384=VECTOR('',#1150,1.);
#385=VECTOR('',#1151,1.);
#386=VECTOR('',#1152,1.);
#387=VECTOR('',#1155,1.);
#388=VECTOR('',#1156,1.);
#389=VECTOR('',#1159,1.);
#390=VECTOR('',#1160,1.);
#391=VECTOR('',#1161,1.);
#392=VECTOR('',#1162,1.);
#393=VECTOR('',#1165,1.);
#394=VECTOR('',#1166,1.);
#395=VECTOR('',#1167,1.);
#396=VECTOR('',#1170,1.);
#397=VECTOR('',#1171,1.);
#398=VECTOR('',#1172,1.);
#399=VECTOR('',#1175,1.);
#400=VECTOR('',#1176,1.);
#401=VECTOR('',#1187,0.510000000000002);
#402=VECTOR('',#1192,1.);
#403=VECTOR('',#1193,1.);
#404=VECTOR('',#1194,1.);
#405=VECTOR('',#1195,1.);
#406=VECTOR('',#1198,1.);
#407=VECTOR('',#1199,1.);
#408=VECTOR('',#1200,1.);
#409=VECTOR('',#1201,1.);
#410=VECTOR('',#1204,1.);
#411=VECTOR('',#1205,1.);
#412=VECTOR('',#1234,0.515000000000001);
#413=VECTOR('',#1241,0.515000000000001);
#414=VECTOR('',#1246,1.);
#415=VECTOR('',#1247,1.);
#416=VECTOR('',#1248,1.);
#417=VECTOR('',#1249,1.);
#418=VECTOR('',#1252,1.);
#419=VECTOR('',#1253,1.);
#420=VECTOR('',#1254,1.);
#421=VECTOR('',#1257,1.);
#422=VECTOR('',#1258,1.);
#423=VECTOR('',#1259,1.);
#424=VECTOR('',#1262,1.);
#425=VECTOR('',#1263,1.);
#426=VECTOR('',#1264,1.);
#427=VECTOR('',#1267,1.);
#428=VECTOR('',#1268,1.);
#429=VECTOR('',#1269,1.);
#430=VECTOR('',#1272,1.);
#431=VECTOR('',#1273,1.);
#432=VECTOR('',#1274,1.);
#433=VECTOR('',#1277,1.);
#434=VECTOR('',#1278,1.);
#435=VECTOR('',#1279,1.);
#436=VECTOR('',#1282,1.);
#437=VECTOR('',#1283,1.);
#438=VECTOR('',#1294,0.510000000000002);
#439=VECTOR('',#1301,0.899999999999999);
#440=VECTOR('',#1312,0.16);
#441=VECTOR('',#1321,0.875);
#442=VECTOR('',#1326,0.9);
#443=VECTOR('',#1335,0.5);
#444=VECTOR('',#1336,0.5);
#445=VECTOR('',#1341,0.435);
#446=VECTOR('',#1350,0.525);
#447=VECTOR('',#1357,1.);
#448=VECTOR('',#1376,1.);
#449=VECTOR('',#1379,1.);
#450=VECTOR('',#1380,1.);
#451=VECTOR('',#1381,1.);
#452=VECTOR('',#1386,0.16);
#453=VERTEX_POINT('',#1429);
#454=VERTEX_POINT('',#1430);
#455=VERTEX_POINT('',#1432);
#456=VERTEX_POINT('',#1434);
#457=VERTEX_POINT('',#1438);
#458=VERTEX_POINT('',#1440);
#459=VERTEX_POINT('',#1444);
#460=VERTEX_POINT('',#1446);
#461=VERTEX_POINT('',#1453);
#462=VERTEX_POINT('',#1454);
#463=VERTEX_POINT('',#1456);
#464=VERTEX_POINT('',#1458);
#465=VERTEX_POINT('',#1462);
#466=VERTEX_POINT('',#1464);
#467=VERTEX_POINT('',#1468);
#468=VERTEX_POINT('',#1470);
#469=VERTEX_POINT('',#1480);
#470=VERTEX_POINT('',#1482);
#471=VERTEX_POINT('',#1486);
#472=VERTEX_POINT('',#1487);
#473=VERTEX_POINT('',#1489);
#474=VERTEX_POINT('',#1491);
#475=VERTEX_POINT('',#1495);
#476=VERTEX_POINT('',#1496);
#477=VERTEX_POINT('',#1498);
#478=VERTEX_POINT('',#1500);
#479=VERTEX_POINT('',#1519);
#480=VERTEX_POINT('',#1521);
#481=VERTEX_POINT('',#1525);
#482=VERTEX_POINT('',#1527);
#483=VERTEX_POINT('',#1531);
#484=VERTEX_POINT('',#1532);
#485=VERTEX_POINT('',#1534);
#486=VERTEX_POINT('',#1536);
#487=VERTEX_POINT('',#1540);
#488=VERTEX_POINT('',#1542);
#489=VERTEX_POINT('',#1546);
#490=VERTEX_POINT('',#1548);
#491=VERTEX_POINT('',#1552);
#492=VERTEX_POINT('',#1554);
#493=VERTEX_POINT('',#1558);
#494=VERTEX_POINT('',#1560);
#495=VERTEX_POINT('',#1564);
#496=VERTEX_POINT('',#1566);
#497=VERTEX_POINT('',#1570);
#498=VERTEX_POINT('',#1572);
#499=VERTEX_POINT('',#1582);
#500=VERTEX_POINT('',#1584);
#501=VERTEX_POINT('',#1588);
#502=VERTEX_POINT('',#1590);
#503=VERTEX_POINT('',#1597);
#504=VERTEX_POINT('',#1598);
#505=VERTEX_POINT('',#1609);
#506=VERTEX_POINT('',#1645);
#507=VERTEX_POINT('',#1675);
#508=VERTEX_POINT('',#1678);
#509=VERTEX_POINT('',#1682);
#510=VERTEX_POINT('',#1686);
#511=VERTEX_POINT('',#1689);
#512=VERTEX_POINT('',#1694);
#513=VERTEX_POINT('',#1700);
#514=VERTEX_POINT('',#1702);
#515=VERTEX_POINT('',#1706);
#516=VERTEX_POINT('',#1708);
#517=VERTEX_POINT('',#1715);
#518=VERTEX_POINT('',#1718);
#519=VERTEX_POINT('',#1719);
#520=VERTEX_POINT('',#1773);
#521=VERTEX_POINT('',#1774);
#522=VERTEX_POINT('',#1778);
#523=VERTEX_POINT('',#1780);
#524=VERTEX_POINT('',#1784);
#525=EDGE_CURVE('',#453,#454,#301,.T.);
#526=EDGE_CURVE('',#455,#453,#302,.T.);
#527=EDGE_CURVE('',#456,#455,#303,.T.);
#528=EDGE_CURVE('',#456,#454,#304,.T.);
#529=EDGE_CURVE('',#454,#457,#305,.T.);
#530=EDGE_CURVE('',#458,#456,#306,.T.);
#531=EDGE_CURVE('',#458,#457,#307,.T.);
#532=EDGE_CURVE('',#457,#459,#308,.T.);
#533=EDGE_CURVE('',#460,#458,#309,.T.);
#534=EDGE_CURVE('',#460,#459,#310,.T.);
#535=EDGE_CURVE('',#459,#453,#311,.T.);
#536=EDGE_CURVE('',#455,#460,#312,.T.);
#537=EDGE_CURVE('',#461,#462,#313,.T.);
#538=EDGE_CURVE('',#462,#463,#314,.T.);
#539=EDGE_CURVE('',#464,#463,#315,.T.);
#540=EDGE_CURVE('',#461,#464,#316,.T.);
#541=EDGE_CURVE('',#465,#461,#317,.T.);
#542=EDGE_CURVE('',#466,#464,#318,.T.);
#543=EDGE_CURVE('',#465,#466,#319,.T.);
#544=EDGE_CURVE('',#467,#465,#320,.T.);
#545=EDGE_CURVE('',#468,#466,#321,.T.);
#546=EDGE_CURVE('',#467,#468,#322,.T.);
#547=EDGE_CURVE('',#462,#467,#323,.T.);
#548=EDGE_CURVE('',#463,#468,#324,.T.);
#549=EDGE_CURVE('',#469,#469,#104,.T.);
#550=EDGE_CURVE('',#469,#470,#325,.T.);
#551=EDGE_CURVE('',#470,#470,#105,.T.);
#552=EDGE_CURVE('',#471,#472,#326,.T.);
#553=EDGE_CURVE('',#471,#473,#327,.T.);
#554=EDGE_CURVE('',#474,#473,#328,.T.);
#555=EDGE_CURVE('',#472,#474,#329,.T.);
#556=EDGE_CURVE('',#475,#476,#330,.T.);
#557=EDGE_CURVE('',#477,#475,#331,.T.);
#558=EDGE_CURVE('',#478,#477,#332,.T.);
#559=EDGE_CURVE('',#476,#478,#333,.T.);
#560=EDGE_CURVE('',#473,#478,#334,.T.);
#561=EDGE_CURVE('',#476,#471,#335,.T.);
#562=EDGE_CURVE('',#477,#474,#106,.T.);
#563=EDGE_CURVE('',#475,#472,#107,.T.);
#564=EDGE_CURVE('',#479,#479,#108,.T.);
#565=EDGE_CURVE('',#479,#480,#336,.T.);
#566=EDGE_CURVE('',#480,#480,#109,.T.);
#567=EDGE_CURVE('',#481,#481,#110,.T.);
#568=EDGE_CURVE('',#481,#482,#337,.T.);
#569=EDGE_CURVE('',#482,#482,#111,.T.);
#570=EDGE_CURVE('',#483,#484,#338,.T.);
#571=EDGE_CURVE('',#483,#485,#339,.T.);
#572=EDGE_CURVE('',#486,#485,#340,.T.);
#573=EDGE_CURVE('',#484,#486,#341,.T.);
#574=EDGE_CURVE('',#484,#487,#342,.T.);
#575=EDGE_CURVE('',#488,#486,#343,.T.);
#576=EDGE_CURVE('',#487,#488,#344,.T.);
#577=EDGE_CURVE('',#487,#489,#345,.T.);
#578=EDGE_CURVE('',#490,#488,#346,.T.);
#579=EDGE_CURVE('',#489,#490,#347,.T.);
#580=EDGE_CURVE('',#489,#491,#348,.T.);
#581=EDGE_CURVE('',#492,#490,#349,.T.);
#582=EDGE_CURVE('',#491,#492,#350,.T.);
#583=EDGE_CURVE('',#491,#493,#351,.T.);
#584=EDGE_CURVE('',#494,#492,#352,.T.);
#585=EDGE_CURVE('',#493,#494,#353,.T.);
#586=EDGE_CURVE('',#493,#495,#354,.T.);
#587=EDGE_CURVE('',#496,#494,#355,.T.);
#588=EDGE_CURVE('',#495,#496,#356,.T.);
#589=EDGE_CURVE('',#495,#497,#357,.T.);
#590=EDGE_CURVE('',#498,#496,#358,.T.);
#591=EDGE_CURVE('',#497,#498,#359,.T.);
#592=EDGE_CURVE('',#497,#483,#360,.T.);
#593=EDGE_CURVE('',#485,#498,#361,.T.);
#594=EDGE_CURVE('',#499,#499,#112,.T.);
#595=EDGE_CURVE('',#499,#500,#362,.T.);
#596=EDGE_CURVE('',#500,#500,#113,.T.);
#597=EDGE_CURVE('',#501,#501,#114,.T.);
#598=EDGE_CURVE('',#501,#502,#363,.T.);
#599=EDGE_CURVE('',#502,#502,#115,.T.);
#600=EDGE_CURVE('',#503,#504,#14,.T.);
#601=EDGE_CURVE('',#503,#505,#364,.T.);
#602=EDGE_CURVE('',#505,#505,#15,.T.);
#603=EDGE_CURVE('',#506,#503,#16,.T.);
#604=EDGE_CURVE('',#504,#506,#17,.T.);
#605=EDGE_CURVE('',#507,#507,#116,.T.);
#606=EDGE_CURVE('',#508,#508,#117,.T.);
#607=EDGE_CURVE('',#508,#507,#365,.T.);
#608=EDGE_CURVE('',#509,#509,#118,.T.);
#609=EDGE_CURVE('',#509,#508,#366,.T.);
#610=EDGE_CURVE('',#510,#510,#119,.T.);
#611=EDGE_CURVE('',#511,#511,#120,.T.);
#612=EDGE_CURVE('',#511,#504,#367,.T.);
#613=EDGE_CURVE('',#506,#510,#368,.T.);
#614=EDGE_CURVE('',#512,#512,#121,.T.);
#615=EDGE_CURVE('',#512,#511,#369,.T.);
#616=EDGE_CURVE('',#513,#513,#122,.T.);
#617=EDGE_CURVE('',#513,#514,#370,.T.);
#618=EDGE_CURVE('',#514,#514,#123,.T.);
#619=EDGE_CURVE('',#515,#515,#124,.T.);
#620=EDGE_CURVE('',#515,#516,#371,.T.);
#621=EDGE_CURVE('',#516,#516,#125,.T.);
#622=EDGE_CURVE('',#517,#517,#126,.T.);
#623=EDGE_CURVE('',#517,#517,#127,.T.);
#624=EDGE_CURVE('',#518,#519,#18,.T.);
#625=EDGE_CURVE('',#519,#518,#19,.T.);
#626=EDGE_CURVE('',#520,#521,#128,.T.);
#627=EDGE_CURVE('',#520,#521,#372,.T.);
#628=EDGE_CURVE('',#521,#522,#373,.T.);
#629=EDGE_CURVE('',#523,#522,#374,.T.);
#630=EDGE_CURVE('',#520,#523,#375,.T.);
#631=EDGE_CURVE('',#524,#523,#129,.T.);
#632=EDGE_CURVE('',#524,#519,#376,.T.);
#633=EDGE_CURVE('',#522,#524,#130,.T.);
#634=ORIENTED_EDGE('',*,*,#525,.F.);
#635=ORIENTED_EDGE('',*,*,#526,.F.);
#636=ORIENTED_EDGE('',*,*,#527,.F.);
#637=ORIENTED_EDGE('',*,*,#528,.T.);
#638=ORIENTED_EDGE('',*,*,#529,.F.);
#639=ORIENTED_EDGE('',*,*,#528,.F.);
#640=ORIENTED_EDGE('',*,*,#530,.F.);
#641=ORIENTED_EDGE('',*,*,#531,.T.);
#642=ORIENTED_EDGE('',*,*,#532,.F.);
#643=ORIENTED_EDGE('',*,*,#531,.F.);
#644=ORIENTED_EDGE('',*,*,#533,.F.);
#645=ORIENTED_EDGE('',*,*,#534,.T.);
#646=ORIENTED_EDGE('',*,*,#535,.F.);
#647=ORIENTED_EDGE('',*,*,#534,.F.);
#648=ORIENTED_EDGE('',*,*,#536,.F.);
#649=ORIENTED_EDGE('',*,*,#526,.T.);
#650=ORIENTED_EDGE('',*,*,#537,.T.);
#651=ORIENTED_EDGE('',*,*,#538,.T.);
#652=ORIENTED_EDGE('',*,*,#539,.F.);
#653=ORIENTED_EDGE('',*,*,#540,.F.);
#654=ORIENTED_EDGE('',*,*,#541,.T.);
#655=ORIENTED_EDGE('',*,*,#540,.T.);
#656=ORIENTED_EDGE('',*,*,#542,.F.);
#657=ORIENTED_EDGE('',*,*,#543,.F.);
#658=ORIENTED_EDGE('',*,*,#532,.T.);
#659=ORIENTED_EDGE('',*,*,#535,.T.);
#660=ORIENTED_EDGE('',*,*,#525,.T.);
#661=ORIENTED_EDGE('',*,*,#529,.T.);
#662=ORIENTED_EDGE('',*,*,#544,.T.);
#663=ORIENTED_EDGE('',*,*,#543,.T.);
#664=ORIENTED_EDGE('',*,*,#545,.F.);
#665=ORIENTED_EDGE('',*,*,#546,.F.);
#666=ORIENTED_EDGE('',*,*,#547,.T.);
#667=ORIENTED_EDGE('',*,*,#546,.T.);
#668=ORIENTED_EDGE('',*,*,#548,.F.);
#669=ORIENTED_EDGE('',*,*,#538,.F.);
#670=ORIENTED_EDGE('',*,*,#533,.T.);
#671=ORIENTED_EDGE('',*,*,#530,.T.);
#672=ORIENTED_EDGE('',*,*,#527,.T.);
#673=ORIENTED_EDGE('',*,*,#536,.T.);
#674=ORIENTED_EDGE('',*,*,#548,.T.);
#675=ORIENTED_EDGE('',*,*,#545,.T.);
#676=ORIENTED_EDGE('',*,*,#542,.T.);
#677=ORIENTED_EDGE('',*,*,#539,.T.);
#678=ORIENTED_EDGE('',*,*,#547,.F.);
#679=ORIENTED_EDGE('',*,*,#537,.F.);
#680=ORIENTED_EDGE('',*,*,#541,.F.);
#681=ORIENTED_EDGE('',*,*,#544,.F.);
#682=ORIENTED_EDGE('',*,*,#549,.F.);
#683=ORIENTED_EDGE('',*,*,#550,.T.);
#684=ORIENTED_EDGE('',*,*,#551,.F.);
#685=ORIENTED_EDGE('',*,*,#550,.F.);
#686=ORIENTED_EDGE('',*,*,#552,.F.);
#687=ORIENTED_EDGE('',*,*,#553,.T.);
#688=ORIENTED_EDGE('',*,*,#554,.F.);
#689=ORIENTED_EDGE('',*,*,#555,.F.);
#690=ORIENTED_EDGE('',*,*,#556,.F.);
#691=ORIENTED_EDGE('',*,*,#557,.F.);
#692=ORIENTED_EDGE('',*,*,#558,.F.);
#693=ORIENTED_EDGE('',*,*,#559,.F.);
#694=ORIENTED_EDGE('',*,*,#560,.F.);
#695=ORIENTED_EDGE('',*,*,#553,.F.);
#696=ORIENTED_EDGE('',*,*,#561,.F.);
#697=ORIENTED_EDGE('',*,*,#559,.T.);
#698=ORIENTED_EDGE('',*,*,#562,.T.);
#699=ORIENTED_EDGE('',*,*,#554,.T.);
#700=ORIENTED_EDGE('',*,*,#560,.T.);
#701=ORIENTED_EDGE('',*,*,#558,.T.);
#702=ORIENTED_EDGE('',*,*,#551,.T.);
#703=ORIENTED_EDGE('',*,*,#555,.T.);
#704=ORIENTED_EDGE('',*,*,#562,.F.);
#705=ORIENTED_EDGE('',*,*,#557,.T.);
#706=ORIENTED_EDGE('',*,*,#563,.T.);
#707=ORIENTED_EDGE('',*,*,#563,.F.);
#708=ORIENTED_EDGE('',*,*,#556,.T.);
#709=ORIENTED_EDGE('',*,*,#561,.T.);
#710=ORIENTED_EDGE('',*,*,#552,.T.);
#711=ORIENTED_EDGE('',*,*,#549,.T.);
#712=ORIENTED_EDGE('',*,*,#564,.F.);
#713=ORIENTED_EDGE('',*,*,#565,.T.);
#714=ORIENTED_EDGE('',*,*,#566,.F.);
#715=ORIENTED_EDGE('',*,*,#565,.F.);
#716=ORIENTED_EDGE('',*,*,#567,.F.);
#717=ORIENTED_EDGE('',*,*,#568,.T.);
#718=ORIENTED_EDGE('',*,*,#569,.F.);
#719=ORIENTED_EDGE('',*,*,#568,.F.);
#720=ORIENTED_EDGE('',*,*,#570,.F.);
#721=ORIENTED_EDGE('',*,*,#571,.T.);
#722=ORIENTED_EDGE('',*,*,#572,.F.);
#723=ORIENTED_EDGE('',*,*,#573,.F.);
#724=ORIENTED_EDGE('',*,*,#567,.T.);
#725=ORIENTED_EDGE('',*,*,#574,.F.);
#726=ORIENTED_EDGE('',*,*,#573,.T.);
#727=ORIENTED_EDGE('',*,*,#575,.F.);
#728=ORIENTED_EDGE('',*,*,#576,.F.);
#729=ORIENTED_EDGE('',*,*,#577,.F.);
#730=ORIENTED_EDGE('',*,*,#576,.T.);
#731=ORIENTED_EDGE('',*,*,#578,.F.);
#732=ORIENTED_EDGE('',*,*,#579,.F.);
#733=ORIENTED_EDGE('',*,*,#569,.T.);
#734=ORIENTED_EDGE('',*,*,#580,.F.);
#735=ORIENTED_EDGE('',*,*,#579,.T.);
#736=ORIENTED_EDGE('',*,*,#581,.F.);
#737=ORIENTED_EDGE('',*,*,#582,.F.);
#738=ORIENTED_EDGE('',*,*,#583,.F.);
#739=ORIENTED_EDGE('',*,*,#582,.T.);
#740=ORIENTED_EDGE('',*,*,#584,.F.);
#741=ORIENTED_EDGE('',*,*,#585,.F.);
#742=ORIENTED_EDGE('',*,*,#564,.T.);
#743=ORIENTED_EDGE('',*,*,#586,.F.);
#744=ORIENTED_EDGE('',*,*,#585,.T.);
#745=ORIENTED_EDGE('',*,*,#587,.F.);
#746=ORIENTED_EDGE('',*,*,#588,.F.);
#747=ORIENTED_EDGE('',*,*,#589,.F.);
#748=ORIENTED_EDGE('',*,*,#588,.T.);
#749=ORIENTED_EDGE('',*,*,#590,.F.);
#750=ORIENTED_EDGE('',*,*,#591,.F.);
#751=ORIENTED_EDGE('',*,*,#566,.T.);
#752=ORIENTED_EDGE('',*,*,#592,.F.);
#753=ORIENTED_EDGE('',*,*,#591,.T.);
#754=ORIENTED_EDGE('',*,*,#593,.F.);
#755=ORIENTED_EDGE('',*,*,#571,.F.);
#756=ORIENTED_EDGE('',*,*,#593,.T.);
#757=ORIENTED_EDGE('',*,*,#590,.T.);
#758=ORIENTED_EDGE('',*,*,#587,.T.);
#759=ORIENTED_EDGE('',*,*,#584,.T.);
#760=ORIENTED_EDGE('',*,*,#581,.T.);
#761=ORIENTED_EDGE('',*,*,#578,.T.);
#762=ORIENTED_EDGE('',*,*,#575,.T.);
#763=ORIENTED_EDGE('',*,*,#572,.T.);
#764=ORIENTED_EDGE('',*,*,#592,.T.);
#765=ORIENTED_EDGE('',*,*,#570,.T.);
#766=ORIENTED_EDGE('',*,*,#574,.T.);
#767=ORIENTED_EDGE('',*,*,#577,.T.);
#768=ORIENTED_EDGE('',*,*,#580,.T.);
#769=ORIENTED_EDGE('',*,*,#583,.T.);
#770=ORIENTED_EDGE('',*,*,#586,.T.);
#771=ORIENTED_EDGE('',*,*,#589,.T.);
#772=ORIENTED_EDGE('',*,*,#594,.F.);
#773=ORIENTED_EDGE('',*,*,#595,.T.);
#774=ORIENTED_EDGE('',*,*,#596,.T.);
#775=ORIENTED_EDGE('',*,*,#595,.F.);
#776=ORIENTED_EDGE('',*,*,#597,.F.);
#777=ORIENTED_EDGE('',*,*,#598,.T.);
#778=ORIENTED_EDGE('',*,*,#599,.T.);
#779=ORIENTED_EDGE('',*,*,#598,.F.);
#780=ORIENTED_EDGE('',*,*,#597,.T.);
#781=ORIENTED_EDGE('',*,*,#594,.T.);
#782=ORIENTED_EDGE('',*,*,#599,.F.);
#783=ORIENTED_EDGE('',*,*,#596,.F.);
#784=ORIENTED_EDGE('',*,*,#600,.F.);
#785=ORIENTED_EDGE('',*,*,#601,.T.);
#786=ORIENTED_EDGE('',*,*,#602,.F.);
#787=ORIENTED_EDGE('',*,*,#601,.F.);
#788=ORIENTED_EDGE('',*,*,#603,.F.);
#789=ORIENTED_EDGE('',*,*,#604,.F.);
#790=ORIENTED_EDGE('',*,*,#605,.F.);
#791=ORIENTED_EDGE('',*,*,#606,.F.);
#792=ORIENTED_EDGE('',*,*,#607,.T.);
#793=ORIENTED_EDGE('',*,*,#605,.T.);
#794=ORIENTED_EDGE('',*,*,#607,.F.);
#795=ORIENTED_EDGE('',*,*,#608,.F.);
#796=ORIENTED_EDGE('',*,*,#609,.T.);
#797=ORIENTED_EDGE('',*,*,#606,.T.);
#798=ORIENTED_EDGE('',*,*,#609,.F.);
#799=ORIENTED_EDGE('',*,*,#608,.T.);
#800=ORIENTED_EDGE('',*,*,#610,.F.);
#801=ORIENTED_EDGE('',*,*,#611,.F.);
#802=ORIENTED_EDGE('',*,*,#612,.T.);
#803=ORIENTED_EDGE('',*,*,#604,.T.);
#804=ORIENTED_EDGE('',*,*,#613,.T.);
#805=ORIENTED_EDGE('',*,*,#610,.T.);
#806=ORIENTED_EDGE('',*,*,#613,.F.);
#807=ORIENTED_EDGE('',*,*,#603,.T.);
#808=ORIENTED_EDGE('',*,*,#600,.T.);
#809=ORIENTED_EDGE('',*,*,#612,.F.);
#810=ORIENTED_EDGE('',*,*,#602,.T.);
#811=ORIENTED_EDGE('',*,*,#614,.F.);
#812=ORIENTED_EDGE('',*,*,#615,.T.);
#813=ORIENTED_EDGE('',*,*,#611,.T.);
#814=ORIENTED_EDGE('',*,*,#615,.F.);
#815=ORIENTED_EDGE('',*,*,#614,.T.);
#816=ORIENTED_EDGE('',*,*,#616,.F.);
#817=ORIENTED_EDGE('',*,*,#617,.T.);
#818=ORIENTED_EDGE('',*,*,#618,.T.);
#819=ORIENTED_EDGE('',*,*,#617,.F.);
#820=ORIENTED_EDGE('',*,*,#619,.F.);
#821=ORIENTED_EDGE('',*,*,#620,.T.);
#822=ORIENTED_EDGE('',*,*,#621,.T.);
#823=ORIENTED_EDGE('',*,*,#620,.F.);
#824=ORIENTED_EDGE('',*,*,#619,.T.);
#825=ORIENTED_EDGE('',*,*,#616,.T.);
#826=ORIENTED_EDGE('',*,*,#621,.F.);
#827=ORIENTED_EDGE('',*,*,#618,.F.);
#828=ORIENTED_EDGE('',*,*,#622,.F.);
#829=ORIENTED_EDGE('',*,*,#623,.T.);
#830=ORIENTED_EDGE('',*,*,#622,.T.);
#831=ORIENTED_EDGE('',*,*,#623,.F.);
#832=ORIENTED_EDGE('',*,*,#624,.F.);
#833=ORIENTED_EDGE('',*,*,#625,.F.);
#834=ORIENTED_EDGE('',*,*,#626,.T.);
#835=ORIENTED_EDGE('',*,*,#627,.F.);
#836=ORIENTED_EDGE('',*,*,#627,.T.);
#837=ORIENTED_EDGE('',*,*,#628,.T.);
#838=ORIENTED_EDGE('',*,*,#629,.F.);
#839=ORIENTED_EDGE('',*,*,#630,.F.);
#840=ORIENTED_EDGE('',*,*,#626,.F.);
#841=ORIENTED_EDGE('',*,*,#630,.T.);
#842=ORIENTED_EDGE('',*,*,#631,.F.);
#843=ORIENTED_EDGE('',*,*,#632,.T.);
#844=ORIENTED_EDGE('',*,*,#625,.T.);
#845=ORIENTED_EDGE('',*,*,#624,.T.);
#846=ORIENTED_EDGE('',*,*,#632,.F.);
#847=ORIENTED_EDGE('',*,*,#633,.F.);
#848=ORIENTED_EDGE('',*,*,#628,.F.);
#849=ORIENTED_EDGE('',*,*,#633,.T.);
#850=ORIENTED_EDGE('',*,*,#631,.T.);
#851=ORIENTED_EDGE('',*,*,#629,.T.);
#852=PLANE('',#1025);
#853=PLANE('',#1026);
#854=PLANE('',#1027);
#855=PLANE('',#1028);
#856=PLANE('',#1029);
#857=PLANE('',#1030);
#858=PLANE('',#1031);
#859=PLANE('',#1032);
#860=PLANE('',#1033);
#861=PLANE('',#1034);
#862=PLANE('',#1039);
#863=PLANE('',#1040);
#864=PLANE('',#1041);
#865=PLANE('',#1042);
#866=PLANE('',#1046);
#867=PLANE('',#1060);
#868=PLANE('',#1061);
#869=PLANE('',#1062);
#870=PLANE('',#1063);
#871=PLANE('',#1064);
#872=PLANE('',#1065);
#873=PLANE('',#1066);
#874=PLANE('',#1067);
#875=PLANE('',#1068);
#876=PLANE('',#1069);
#877=PLANE('',#1077);
#878=PLANE('',#1078);
#879=PLANE('',#1081);
#880=PLANE('',#1087);
#881=PLANE('',#1093);
#882=PLANE('',#1101);
#883=PLANE('',#1102);
#884=PLANE('',#1107);
#885=PLANE('',#1109);
#886=PLANE('',#1113);
#887=ADVANCED_FACE('',(#186),#852,.F.);
#888=ADVANCED_FACE('',(#187),#853,.F.);
#889=ADVANCED_FACE('',(#188),#854,.F.);
#890=ADVANCED_FACE('',(#189),#855,.F.);
#891=ADVANCED_FACE('',(#190),#856,.T.);
#892=ADVANCED_FACE('',(#191,#171),#857,.T.);
#893=ADVANCED_FACE('',(#192),#858,.T.);
#894=ADVANCED_FACE('',(#193,#172),#859,.T.);
#895=ADVANCED_FACE('',(#194),#860,.T.);
#896=ADVANCED_FACE('',(#195),#861,.F.);
#897=ADVANCED_FACE('',(#196),#131,.F.);
#898=ADVANCED_FACE('',(#197),#862,.T.);
#899=ADVANCED_FACE('',(#198),#863,.T.);
#900=ADVANCED_FACE('',(#199),#864,.T.);
#901=ADVANCED_FACE('',(#200,#173),#865,.T.);
#902=ADVANCED_FACE('',(#201),#132,.T.);
#903=ADVANCED_FACE('',(#202,#174),#866,.F.);
#904=ADVANCED_FACE('',(#203),#133,.F.);
#905=ADVANCED_FACE('',(#204),#134,.F.);
#906=ADVANCED_FACE('',(#205,#175),#867,.T.);
#907=ADVANCED_FACE('',(#206),#868,.T.);
#908=ADVANCED_FACE('',(#207,#176),#869,.T.);
#909=ADVANCED_FACE('',(#208),#870,.T.);
#910=ADVANCED_FACE('',(#209,#177),#871,.T.);
#911=ADVANCED_FACE('',(#210),#872,.T.);
#912=ADVANCED_FACE('',(#211,#178),#873,.T.);
#913=ADVANCED_FACE('',(#212),#874,.T.);
#914=ADVANCED_FACE('',(#213),#875,.T.);
#915=ADVANCED_FACE('',(#214),#876,.F.);
#916=ADVANCED_FACE('',(#215),#135,.F.);
#917=ADVANCED_FACE('',(#216),#136,.T.);
#918=ADVANCED_FACE('',(#217,#179),#877,.T.);
#919=ADVANCED_FACE('',(#218,#180),#878,.F.);
#920=ADVANCED_FACE('',(#219),#137,.F.);
#921=ADVANCED_FACE('',(#220),#879,.T.);
#922=ADVANCED_FACE('',(#221),#12,.T.);
#923=ADVANCED_FACE('',(#222),#138,.T.);
#924=ADVANCED_FACE('',(#223,#181),#880,.T.);
#925=ADVANCED_FACE('',(#224,#182),#139,.T.);
#926=ADVANCED_FACE('',(#225),#13,.T.);
#927=ADVANCED_FACE('',(#226),#881,.T.);
#928=ADVANCED_FACE('',(#227),#140,.F.);
#929=ADVANCED_FACE('',(#228),#141,.T.);
#930=ADVANCED_FACE('',(#229,#183),#882,.T.);
#931=ADVANCED_FACE('',(#230,#184),#883,.F.);
#932=ADVANCED_FACE('',(#231,#185),#11,.T.);
#933=ADVANCED_FACE('',(#232),#884,.F.);
#934=ADVANCED_FACE('',(#233),#885,.T.);
#935=ADVANCED_FACE('',(#234),#142,.T.);
#936=ADVANCED_FACE('',(#235),#886,.F.);
#937=CLOSED_SHELL('',(#887,#888,#889,#890,#891,#892,#893,#894,#895,#896));
#938=CLOSED_SHELL('',(#897,#898,#899,#900,#901,#902,#903));
#939=CLOSED_SHELL('',(#904,#905,#906,#907,#908,#909,#910,#911,#912,#913,
#914,#915));
#940=CLOSED_SHELL('',(#916,#917,#918,#919));
#941=CLOSED_SHELL('',(#920,#921,#922,#923,#924,#925,#926,#927));
#942=CLOSED_SHELL('',(#928,#929,#930,#931));
#943=CLOSED_SHELL('',(#932,#933,#934,#935,#936));
#944=DERIVED_UNIT_ELEMENT(#958,1.);
#945=DERIVED_UNIT_ELEMENT(#1831,-3.);
#946=DERIVED_UNIT_ELEMENT(#958,1.);
#947=DERIVED_UNIT_ELEMENT(#1831,-3.);
#948=DERIVED_UNIT_ELEMENT(#958,1.);
#949=DERIVED_UNIT_ELEMENT(#1831,-3.);
#950=DERIVED_UNIT_ELEMENT(#958,1.);
#951=DERIVED_UNIT_ELEMENT(#1831,-3.);
#952=DERIVED_UNIT_ELEMENT(#958,1.);
#953=DERIVED_UNIT_ELEMENT(#1831,-3.);
#954=DERIVED_UNIT_ELEMENT(#958,1.);
#955=DERIVED_UNIT_ELEMENT(#1831,-3.);
#956=DERIVED_UNIT_ELEMENT(#958,1.);
#957=DERIVED_UNIT_ELEMENT(#1831,-3.);
#958=(
MASS_UNIT()
NAMED_UNIT(*)
SI_UNIT(.KILO.,.GRAM.)
);
#959=DERIVED_UNIT((#944,#945));
#960=DERIVED_UNIT((#946,#947));
#961=DERIVED_UNIT((#948,#949));
#962=DERIVED_UNIT((#950,#951));
#963=DERIVED_UNIT((#952,#953));
#964=DERIVED_UNIT((#954,#955));
#965=DERIVED_UNIT((#956,#957));
#966=MEASURE_REPRESENTATION_ITEM('density measure',
POSITIVE_RATIO_MEASURE(7850.),#959);
#967=MEASURE_REPRESENTATION_ITEM('density measure',
POSITIVE_RATIO_MEASURE(7850.),#960);
#968=MEASURE_REPRESENTATION_ITEM('density measure',
POSITIVE_RATIO_MEASURE(7850.),#961);
#969=MEASURE_REPRESENTATION_ITEM('density measure',
POSITIVE_RATIO_MEASURE(7850.),#962);
#970=MEASURE_REPRESENTATION_ITEM('density measure',
POSITIVE_RATIO_MEASURE(7850.),#963);
#971=MEASURE_REPRESENTATION_ITEM('density measure',
POSITIVE_RATIO_MEASURE(7850.),#964);
#972=MEASURE_REPRESENTATION_ITEM('density measure',
POSITIVE_RATIO_MEASURE(7850.),#965);
#973=PROPERTY_DEFINITION_REPRESENTATION(#1008,#987);
#974=PROPERTY_DEFINITION_REPRESENTATION(#1009,#988);
#975=PROPERTY_DEFINITION_REPRESENTATION(#1010,#989);
#976=PROPERTY_DEFINITION_REPRESENTATION(#1011,#990);
#977=PROPERTY_DEFINITION_REPRESENTATION(#1012,#991);
#978=PROPERTY_DEFINITION_REPRESENTATION(#1013,#992);
#979=PROPERTY_DEFINITION_REPRESENTATION(#1014,#993);
#980=PROPERTY_DEFINITION_REPRESENTATION(#1015,#994);
#981=PROPERTY_DEFINITION_REPRESENTATION(#1016,#995);
#982=PROPERTY_DEFINITION_REPRESENTATION(#1017,#996);
#983=PROPERTY_DEFINITION_REPRESENTATION(#1018,#997);
#984=PROPERTY_DEFINITION_REPRESENTATION(#1019,#998);
#985=PROPERTY_DEFINITION_REPRESENTATION(#1020,#999);
#986=PROPERTY_DEFINITION_REPRESENTATION(#1021,#1000);
#987=REPRESENTATION('material name',(#1001),#1820);
#988=REPRESENTATION('density',(#966),#1820);
#989=REPRESENTATION('material name',(#1002),#1821);
#990=REPRESENTATION('density',(#967),#1821);
#991=REPRESENTATION('material name',(#1003),#1824);
#992=REPRESENTATION('density',(#968),#1824);
#993=REPRESENTATION('material name',(#1004),#1825);
#994=REPRESENTATION('density',(#969),#1825);
#995=REPRESENTATION('material name',(#1005),#1826);
#996=REPRESENTATION('density',(#970),#1826);
#997=REPRESENTATION('material name',(#1006),#1827);
#998=REPRESENTATION('density',(#971),#1827);
#999=REPRESENTATION('material name',(#1007),#1828);
#1000=REPRESENTATION('density',(#972),#1828);
#1001=DESCRIPTIVE_REPRESENTATION_ITEM('Steel','Steel');
#1002=DESCRIPTIVE_REPRESENTATION_ITEM('Steel','Steel');
#1003=DESCRIPTIVE_REPRESENTATION_ITEM('Steel','Steel');
#1004=DESCRIPTIVE_REPRESENTATION_ITEM('Steel','Steel');
#1005=DESCRIPTIVE_REPRESENTATION_ITEM('Steel','Steel');
#1006=DESCRIPTIVE_REPRESENTATION_ITEM('Steel','Steel');
#1007=DESCRIPTIVE_REPRESENTATION_ITEM('Steel','Steel');
#1008=PROPERTY_DEFINITION('material property','material name',#1891);
#1009=PROPERTY_DEFINITION('material property','density of part',#1891);
#1010=PROPERTY_DEFINITION('material property','material name',#1892);
#1011=PROPERTY_DEFINITION('material property','density of part',#1892);
#1012=PROPERTY_DEFINITION('material property','material name',#1895);
#1013=PROPERTY_DEFINITION('material property','density of part',#1895);
#1014=PROPERTY_DEFINITION('material property','material name',#1896);
#1015=PROPERTY_DEFINITION('material property','density of part',#1896);
#1016=PROPERTY_DEFINITION('material property','material name',#1897);
#1017=PROPERTY_DEFINITION('material property','density of part',#1897);
#1018=PROPERTY_DEFINITION('material property','material name',#1898);
#1019=PROPERTY_DEFINITION('material property','density of part',#1898);
#1020=PROPERTY_DEFINITION('material property','material name',#1899);
#1021=PROPERTY_DEFINITION('material property','density of part',#1899);
#1022=AXIS2_PLACEMENT_3D('',#1425,#1131,#1132);
#1023=AXIS2_PLACEMENT_3D('',#1426,#1133,#1134);
#1024=AXIS2_PLACEMENT_3D('',#1427,#1135,#1136);
#1025=AXIS2_PLACEMENT_3D('',#1428,#1137,#1138);
#1026=AXIS2_PLACEMENT_3D('',#1437,#1143,#1144);
#1027=AXIS2_PLACEMENT_3D('',#1443,#1148,#1149);
#1028=AXIS2_PLACEMENT_3D('',#1449,#1153,#1154);
#1029=AXIS2_PLACEMENT_3D('',#1452,#1157,#1158);
#1030=AXIS2_PLACEMENT_3D('',#1461,#1163,#1164);
#1031=AXIS2_PLACEMENT_3D('',#1467,#1168,#1169);
#1032=AXIS2_PLACEMENT_3D('',#1473,#1173,#1174);
#1033=AXIS2_PLACEMENT_3D('',#1476,#1177,#1178);
#1034=AXIS2_PLACEMENT_3D('',#1477,#1179,#1180);
#1035=AXIS2_PLACEMENT_3D('',#1478,#1181,#1182);
#1036=AXIS2_PLACEMENT_3D('',#1479,#1183,#1184);
#1037=AXIS2_PLACEMENT_3D('',#1481,#1185,#1186);
#1038=AXIS2_PLACEMENT_3D('',#1484,#1188,#1189);
#1039=AXIS2_PLACEMENT_3D('',#1485,#1190,#1191);
#1040=AXIS2_PLACEMENT_3D('',#1494,#1196,#1197);
#1041=AXIS2_PLACEMENT_3D('',#1503,#1202,#1203);
#1042=AXIS2_PLACEMENT_3D('',#1506,#1206,#1207);
#1043=AXIS2_PLACEMENT_3D('',#1507,#1208,#1209);
#1044=AXIS2_PLACEMENT_3D('',#1508,#1210,#1211);
#1045=AXIS2_PLACEMENT_3D('',#1509,#1212,#1213);
#1046=AXIS2_PLACEMENT_3D('',#1510,#1214,#1215);
#1047=AXIS2_PLACEMENT_3D('',#1511,#1216,#1217);
#1048=AXIS2_PLACEMENT_3D('',#1512,#1218,#1219);
#1049=AXIS2_PLACEMENT_3D('',#1513,#1220,#1221);
#1050=AXIS2_PLACEMENT_3D('',#1514,#1222,#1223);
#1051=AXIS2_PLACEMENT_3D('',#1515,#1224,#1225);
#1052=AXIS2_PLACEMENT_3D('',#1516,#1226,#1227);
#1053=AXIS2_PLACEMENT_3D('',#1517,#1228,#1229);
#1054=AXIS2_PLACEMENT_3D('',#1518,#1230,#1231);
#1055=AXIS2_PLACEMENT_3D('',#1520,#1232,#1233);
#1056=AXIS2_PLACEMENT_3D('',#1523,#1235,#1236);
#1057=AXIS2_PLACEMENT_3D('',#1524,#1237,#1238);
#1058=AXIS2_PLACEMENT_3D('',#1526,#1239,#1240);
#1059=AXIS2_PLACEMENT_3D('',#1529,#1242,#1243);
#1060=AXIS2_PLACEMENT_3D('',#1530,#1244,#1245);
#1061=AXIS2_PLACEMENT_3D('',#1539,#1250,#1251);
#1062=AXIS2_PLACEMENT_3D('',#1545,#1255,#1256);
#1063=AXIS2_PLACEMENT_3D('',#1551,#1260,#1261);
#1064=AXIS2_PLACEMENT_3D('',#1557,#1265,#1266);
#1065=AXIS2_PLACEMENT_3D('',#1563,#1270,#1271);
#1066=AXIS2_PLACEMENT_3D('',#1569,#1275,#1276);
#1067=AXIS2_PLACEMENT_3D('',#1575,#1280,#1281);
#1068=AXIS2_PLACEMENT_3D('',#1578,#1284,#1285);
#1069=AXIS2_PLACEMENT_3D('',#1579,#1286,#1287);
#1070=AXIS2_PLACEMENT_3D('',#1580,#1288,#1289);
#1071=AXIS2_PLACEMENT_3D('',#1581,#1290,#1291);
#1072=AXIS2_PLACEMENT_3D('',#1583,#1292,#1293);
#1073=AXIS2_PLACEMENT_3D('',#1586,#1295,#1296);
#1074=AXIS2_PLACEMENT_3D('',#1587,#1297,#1298);
#1075=AXIS2_PLACEMENT_3D('',#1589,#1299,#1300);
#1076=AXIS2_PLACEMENT_3D('',#1592,#1302,#1303);
#1077=AXIS2_PLACEMENT_3D('',#1593,#1304,#1305);
#1078=AXIS2_PLACEMENT_3D('',#1594,#1306,#1307);
#1079=AXIS2_PLACEMENT_3D('',#1595,#1308,#1309);
#1080=AXIS2_PLACEMENT_3D('',#1596,#1310,#1311);
#1081=AXIS2_PLACEMENT_3D('',#1674,#1313,#1314);
#1082=AXIS2_PLACEMENT_3D('',#1676,#1315,#1316);
#1083=AXIS2_PLACEMENT_3D('',#1677,#1317,#1318);
#1084=AXIS2_PLACEMENT_3D('',#1679,#1319,#1320);
#1085=AXIS2_PLACEMENT_3D('',#1681,#1322,#1323);
#1086=AXIS2_PLACEMENT_3D('',#1683,#1324,#1325);
#1087=AXIS2_PLACEMENT_3D('',#1685,#1327,#1328);
#1088=AXIS2_PLACEMENT_3D('',#1687,#1329,#1330);
#1089=AXIS2_PLACEMENT_3D('',#1688,#1331,#1332);
#1090=AXIS2_PLACEMENT_3D('',#1690,#1333,#1334);
#1091=AXIS2_PLACEMENT_3D('',#1693,#1337,#1338);
#1092=AXIS2_PLACEMENT_3D('',#1695,#1339,#1340);
#1093=AXIS2_PLACEMENT_3D('',#1697,#1342,#1343);
#1094=AXIS2_PLACEMENT_3D('',#1698,#1344,#1345);
#1095=AXIS2_PLACEMENT_3D('',#1699,#1346,#1347);
#1096=AXIS2_PLACEMENT_3D('',#1701,#1348,#1349);
#1097=AXIS2_PLACEMENT_3D('',#1704,#1351,#1352);
#1098=AXIS2_PLACEMENT_3D('',#1705,#1353,#1354);
#1099=AXIS2_PLACEMENT_3D('',#1707,#1355,#1356);
#1100=AXIS2_PLACEMENT_3D('',#1710,#1358,#1359);
#1101=AXIS2_PLACEMENT_3D('',#1711,#1360,#1361);
#1102=AXIS2_PLACEMENT_3D('',#1712,#1362,#1363);
#1103=AXIS2_PLACEMENT_3D('',#1713,#1364,#1365);
#1104=AXIS2_PLACEMENT_3D('',#1714,#1366,#1367);
#1105=AXIS2_PLACEMENT_3D('',#1716,#1368,#1369);
#1106=AXIS2_PLACEMENT_3D('',#1717,#1370,#1371);
#1107=AXIS2_PLACEMENT_3D('',#1772,#1372,#1373);
#1108=AXIS2_PLACEMENT_3D('',#1775,#1374,#1375);
#1109=AXIS2_PLACEMENT_3D('',#1777,#1377,#1378);
#1110=AXIS2_PLACEMENT_3D('',#1783,#1382,#1383);
#1111=AXIS2_PLACEMENT_3D('',#1785,#1384,#1385);
#1112=AXIS2_PLACEMENT_3D('',#1787,#1387,#1388);
#1113=AXIS2_PLACEMENT_3D('',#1788,#1389,#1390);
#1114=AXIS2_PLACEMENT_3D('',#1789,#1391,#1392);
#1115=AXIS2_PLACEMENT_3D('',#1790,#1393,#1394);
#1116=AXIS2_PLACEMENT_3D('',#1791,#1395,#1396);
#1117=AXIS2_PLACEMENT_3D('',#1792,#1397,#1398);
#1118=AXIS2_PLACEMENT_3D('',#1793,#1399,#1400);
#1119=AXIS2_PLACEMENT_3D('',#1794,#1401,#1402);
#1120=AXIS2_PLACEMENT_3D('',#1795,#1403,#1404);
#1121=AXIS2_PLACEMENT_3D('',#1796,#1405,#1406);
#1122=AXIS2_PLACEMENT_3D('',#1797,#1407,#1408);
#1123=AXIS2_PLACEMENT_3D('',#1798,#1409,#1410);
#1124=AXIS2_PLACEMENT_3D('',#1799,#1411,#1412);
#1125=AXIS2_PLACEMENT_3D('',#1800,#1413,#1414);
#1126=AXIS2_PLACEMENT_3D('',#1801,#1415,#1416);
#1127=AXIS2_PLACEMENT_3D('',#1802,#1417,#1418);
#1128=AXIS2_PLACEMENT_3D('',#1803,#1419,#1420);
#1129=AXIS2_PLACEMENT_3D('',#1804,#1421,#1422);
#1130=AXIS2_PLACEMENT_3D('',#1805,#1423,#1424);
#1131=DIRECTION('axis',(0.,0.,1.));
#1132=DIRECTION('refdir',(1.,0.,0.));
#1133=DIRECTION('axis',(0.,0.,1.));
#1134=DIRECTION('refdir',(1.,0.,0.));
#1135=DIRECTION('axis',(0.,0.,1.));
#1136=DIRECTION('refdir',(1.,0.,0.));
#1137=DIRECTION('center_axis',(0.,0.,-1.));
#1138=DIRECTION('ref_axis',(0.,1.,0.));
#1139=DIRECTION('',(0.,-1.,0.));
#1140=DIRECTION('',(1.,0.,0.));
#1141=DIRECTION('',(0.,1.,0.));
#1142=DIRECTION('',(1.,0.,0.));
#1143=DIRECTION('center_axis',(0.,-1.,0.));
#1144=DIRECTION('ref_axis',(0.,0.,-1.));
#1145=DIRECTION('',(0.,0.,1.));
#1146=DIRECTION('',(0.,0.,-1.));
#1147=DIRECTION('',(1.,0.,0.));
#1148=DIRECTION('center_axis',(0.,0.,1.));
#1149=DIRECTION('ref_axis',(0.,-1.,0.));
#1150=DIRECTION('',(0.,1.,0.));
#1151=DIRECTION('',(0.,-1.,0.));
#1152=DIRECTION('',(1.,0.,0.));
#1153=DIRECTION('center_axis',(0.,1.,0.));
#1154=DIRECTION('ref_axis',(0.,0.,1.));
#1155=DIRECTION('',(0.,0.,-1.));
#1156=DIRECTION('',(0.,0.,1.));
#1157=DIRECTION('center_axis',(0.,1.,0.));
#1158=DIRECTION('ref_axis',(-1.,0.,0.));
#1159=DIRECTION('',(-1.,0.,0.));
#1160=DIRECTION('',(0.,0.,1.));
#1161=DIRECTION('',(-1.,0.,0.));
#1162=DIRECTION('',(0.,0.,1.));
#1163=DIRECTION('center_axis',(1.,0.,0.));
#1164=DIRECTION('ref_axis',(0.,1.,0.));
#1165=DIRECTION('',(0.,1.,0.));
#1166=DIRECTION('',(0.,1.,0.));
#1167=DIRECTION('',(0.,0.,1.));
#1168=DIRECTION('center_axis',(0.,-1.,0.));
#1169=DIRECTION('ref_axis',(1.,0.,0.));
#1170=DIRECTION('',(1.,0.,0.));
#1171=DIRECTION('',(1.,0.,0.));
#1172=DIRECTION('',(0.,0.,1.));
#1173=DIRECTION('center_axis',(-1.,0.,0.));
#1174=DIRECTION('ref_axis',(0.,-1.,0.));
#1175=DIRECTION('',(0.,-1.,0.));
#1176=DIRECTION('',(0.,-1.,0.));
#1177=DIRECTION('center_axis',(0.,0.,1.));
#1178=DIRECTION('ref_axis',(1.,0.,0.));
#1179=DIRECTION('center_axis',(0.,0.,1.));
#1180=DIRECTION('ref_axis',(1.,0.,0.));
#1181=DIRECTION('axis',(0.,0.,1.));
#1182=DIRECTION('refdir',(1.,0.,0.));
#1183=DIRECTION('center_axis',(0.,1.,0.));
#1184=DIRECTION('ref_axis',(1.,0.,0.));
#1185=DIRECTION('center_axis',(0.,1.,0.));
#1186=DIRECTION('ref_axis',(1.,0.,0.));
#1187=DIRECTION('',(0.,1.,0.));
#1188=DIRECTION('center_axis',(0.,-1.,0.));
#1189=DIRECTION('ref_axis',(1.,0.,0.));
#1190=DIRECTION('center_axis',(-1.,0.,0.));
#1191=DIRECTION('ref_axis',(0.,0.,1.));
#1192=DIRECTION('',(0.,0.,-1.));
#1193=DIRECTION('',(0.,1.,0.));
#1194=DIRECTION('',(0.,0.,1.));
#1195=DIRECTION('',(0.,1.,0.));
#1196=DIRECTION('center_axis',(1.,0.,0.));
#1197=DIRECTION('ref_axis',(0.,0.,-1.));
#1198=DIRECTION('',(0.,0.,1.));
#1199=DIRECTION('',(0.,-1.,0.));
#1200=DIRECTION('',(0.,0.,-1.));
#1201=DIRECTION('',(0.,1.,0.));
#1202=DIRECTION('center_axis',(0.,0.,1.));
#1203=DIRECTION('ref_axis',(1.,0.,0.));
#1204=DIRECTION('',(1.,0.,0.));
#1205=DIRECTION('',(-1.,0.,0.));
#1206=DIRECTION('center_axis',(0.,1.,0.));
#1207=DIRECTION('ref_axis',(1.,0.,0.));
#1208=DIRECTION('center_axis',(0.,1.,0.));
#1209=DIRECTION('ref_axis',(1.,0.,0.));
#1210=DIRECTION('center_axis',(0.,1.,0.));
#1211=DIRECTION('ref_axis',(1.,0.,0.));
#1212=DIRECTION('center_axis',(0.,1.,0.));
#1213=DIRECTION('ref_axis',(1.,0.,0.));
#1214=DIRECTION('center_axis',(0.,1.,0.));
#1215=DIRECTION('ref_axis',(1.,0.,0.));
#1216=DIRECTION('',(0.,0.,1.));
#1217=DIRECTION('',(1.,0.,0.));
#1218=DIRECTION('',(0.,0.,1.));
#1219=DIRECTION('',(1.,0.,0.));
#1220=DIRECTION('',(0.,0.,1.));
#1221=DIRECTION('',(1.,0.,0.));
#1222=DIRECTION('',(0.,-1.22464679914735E-16,-1.));
#1223=DIRECTION('',(1.,0.,0.));
#1224=DIRECTION('axis',(0.,0.,1.));
#1225=DIRECTION('refdir',(1.,0.,0.));
#1226=DIRECTION('axis',(0.,0.,1.));
#1227=DIRECTION('refdir',(1.,0.,0.));
#1228=DIRECTION('axis',(0.,0.,1.));
#1229=DIRECTION('refdir',(1.,0.,0.));
#1230=DIRECTION('center_axis',(0.,1.,0.));
#1231=DIRECTION('ref_axis',(1.,0.,0.));
#1232=DIRECTION('center_axis',(0.,1.,0.));
#1233=DIRECTION('ref_axis',(1.,0.,0.));
#1234=DIRECTION('',(0.,1.,0.));
#1235=DIRECTION('center_axis',(0.,-1.,0.));
#1236=DIRECTION('ref_axis',(1.,0.,0.));
#1237=DIRECTION('center_axis',(0.,1.,0.));
#1238=DIRECTION('ref_axis',(1.,0.,0.));
#1239=DIRECTION('center_axis',(0.,1.,0.));
#1240=DIRECTION('ref_axis',(1.,0.,0.));
#1241=DIRECTION('',(0.,1.,0.));
#1242=DIRECTION('center_axis',(0.,-1.,0.));
#1243=DIRECTION('ref_axis',(1.,0.,0.));
#1244=DIRECTION('center_axis',(0.,-1.,0.));
#1245=DIRECTION('ref_axis',(0.,0.,-1.));
#1246=DIRECTION('',(0.,0.,1.));
#1247=DIRECTION('',(1.,0.,0.));
#1248=DIRECTION('',(0.,0.,-1.));
#1249=DIRECTION('',(1.,0.,0.));
#1250=DIRECTION('center_axis',(0.,0.,1.));
#1251=DIRECTION('ref_axis',(0.,-1.,0.));
#1252=DIRECTION('',(0.,1.,0.));
#1253=DIRECTION('',(0.,-1.,0.));
#1254=DIRECTION('',(1.,0.,0.));
#1255=DIRECTION('center_axis',(0.,1.,0.));
#1256=DIRECTION('ref_axis',(0.,0.,1.));
#1257=DIRECTION('',(0.,0.,-1.));
#1258=DIRECTION('',(0.,0.,1.));
#1259=DIRECTION('',(1.,0.,0.));
#1260=DIRECTION('center_axis',(0.,0.,1.));
#1261=DIRECTION('ref_axis',(0.,-1.,0.));
#1262=DIRECTION('',(0.,1.,0.));
#1263=DIRECTION('',(0.,-1.,0.));
#1264=DIRECTION('',(1.,0.,0.));
#1265=DIRECTION('center_axis',(0.,-1.,0.));
#1266=DIRECTION('ref_axis',(0.,0.,-1.));
#1267=DIRECTION('',(0.,0.,1.));
#1268=DIRECTION('',(0.,0.,-1.));
#1269=DIRECTION('',(1.,0.,0.));
#1270=DIRECTION('center_axis',(0.,0.,1.));
#1271=DIRECTION('ref_axis',(0.,-1.,0.));
#1272=DIRECTION('',(0.,1.,0.));
#1273=DIRECTION('',(0.,-1.,0.));
#1274=DIRECTION('',(1.,0.,0.));
#1275=DIRECTION('center_axis',(0.,1.,0.));
#1276=DIRECTION('ref_axis',(0.,0.,1.));
#1277=DIRECTION('',(0.,0.,-1.));
#1278=DIRECTION('',(0.,0.,1.));
#1279=DIRECTION('',(1.,0.,0.));
#1280=DIRECTION('center_axis',(0.,0.,-1.));
#1281=DIRECTION('ref_axis',(0.,1.,0.));
#1282=DIRECTION('',(0.,-1.,0.));
#1283=DIRECTION('',(0.,1.,0.));
#1284=DIRECTION('center_axis',(1.,0.,0.));
#1285=DIRECTION('ref_axis',(0.,0.,-1.));
#1286=DIRECTION('center_axis',(1.,0.,0.));
#1287=DIRECTION('ref_axis',(0.,0.,-1.));
#1288=DIRECTION('axis',(0.,0.,1.));
#1289=DIRECTION('refdir',(1.,0.,0.));
#1290=DIRECTION('center_axis',(0.,1.,0.));
#1291=DIRECTION('ref_axis',(1.,0.,0.));
#1292=DIRECTION('center_axis',(0.,-1.,0.));
#1293=DIRECTION('ref_axis',(1.,0.,0.));
#1294=DIRECTION('',(0.,-1.,0.));
#1295=DIRECTION('center_axis',(0.,-1.,0.));
#1296=DIRECTION('ref_axis',(1.,0.,0.));
#1297=DIRECTION('center_axis',(0.,1.,0.));
#1298=DIRECTION('ref_axis',(1.,0.,0.));
#1299=DIRECTION('center_axis',(0.,1.,0.));
#1300=DIRECTION('ref_axis',(1.,0.,0.));
#1301=DIRECTION('',(0.,-1.,0.));
#1302=DIRECTION('center_axis',(0.,1.,0.));
#1303=DIRECTION('ref_axis',(1.,0.,0.));
#1304=DIRECTION('center_axis',(0.,1.,0.));
#1305=DIRECTION('ref_axis',(1.,0.,0.));
#1306=DIRECTION('center_axis',(0.,1.,0.));
#1307=DIRECTION('ref_axis',(1.,0.,0.));
#1308=DIRECTION('axis',(0.,0.,1.));
#1309=DIRECTION('refdir',(1.,0.,0.));
#1310=DIRECTION('center_axis',(1.,0.,0.));
#1311=DIRECTION('ref_axis',(0.,0.,-1.));
#1312=DIRECTION('',(1.,0.,0.));
#1313=DIRECTION('center_axis',(0.,1.,0.));
#1314=DIRECTION('ref_axis',(0.,0.,1.));
#1315=DIRECTION('center_axis',(0.,-1.,0.));
#1316=DIRECTION('ref_axis',(1.,0.,0.));
#1317=DIRECTION('center_axis',(0.,-1.,0.));
#1318=DIRECTION('ref_axis',(1.,0.,0.));
#1319=DIRECTION('center_axis',(0.,-1.,0.));
#1320=DIRECTION('ref_axis',(1.,0.,0.));
#1321=DIRECTION('',(0.707106781186548,0.707106781186547,8.65956056235494E-17));
#1322=DIRECTION('center_axis',(0.,-1.,0.));
#1323=DIRECTION('ref_axis',(1.,0.,0.));
#1324=DIRECTION('center_axis',(0.,-1.,0.));
#1325=DIRECTION('ref_axis',(1.,0.,0.));
#1326=DIRECTION('',(0.,1.,0.));
#1327=DIRECTION('center_axis',(0.,-1.,0.));
#1328=DIRECTION('ref_axis',(0.,0.,-1.));
#1329=DIRECTION('center_axis',(0.,-1.,0.));
#1330=DIRECTION('ref_axis',(1.,0.,0.));
#1331=DIRECTION('center_axis',(0.,-1.,0.));
#1332=DIRECTION('ref_axis',(1.,0.,0.));
#1333=DIRECTION('center_axis',(0.,-1.,0.));
#1334=DIRECTION('ref_axis',(1.,0.,0.));
#1335=DIRECTION('',(0.,1.,0.));
#1336=DIRECTION('',(0.,1.,0.));
#1337=DIRECTION('center_axis',(0.,1.,0.));
#1338=DIRECTION('ref_axis',(1.,0.,0.));
#1339=DIRECTION('center_axis',(0.,-1.,0.));
#1340=DIRECTION('ref_axis',(1.,0.,0.));
#1341=DIRECTION('',(-0.707106781186548,0.707106781186547,-8.65956056235493E-17));
#1342=DIRECTION('center_axis',(0.,-1.,0.));
#1343=DIRECTION('ref_axis',(0.,0.,-1.));
#1344=DIRECTION('axis',(0.,0.,1.));
#1345=DIRECTION('refdir',(1.,0.,0.));
#1346=DIRECTION('center_axis',(0.,1.,0.));
#1347=DIRECTION('ref_axis',(1.,0.,0.));
#1348=DIRECTION('center_axis',(0.,-1.,0.));
#1349=DIRECTION('ref_axis',(1.,0.,0.));
#1350=DIRECTION('',(0.,-1.,0.));
#1351=DIRECTION('center_axis',(0.,-1.,0.));
#1352=DIRECTION('ref_axis',(1.,0.,0.));
#1353=DIRECTION('center_axis',(0.,1.,0.));
#1354=DIRECTION('ref_axis',(1.,0.,0.));
#1355=DIRECTION('center_axis',(0.,1.,0.));
#1356=DIRECTION('ref_axis',(1.,0.,0.));
#1357=DIRECTION('',(0.,-1.,0.));
#1358=DIRECTION('center_axis',(0.,1.,0.));
#1359=DIRECTION('ref_axis',(1.,0.,0.));
#1360=DIRECTION('center_axis',(0.,1.,0.));
#1361=DIRECTION('ref_axis',(1.,0.,0.));
#1362=DIRECTION('center_axis',(0.,1.,0.));
#1363=DIRECTION('ref_axis',(1.,0.,0.));
#1364=DIRECTION('axis',(0.,0.,1.));
#1365=DIRECTION('refdir',(1.,0.,0.));
#1366=DIRECTION('center_axis',(-1.,0.,0.));
#1367=DIRECTION('ref_axis',(0.,0.,1.));
#1368=DIRECTION('center_axis',(0.,-1.,1.38777878078145E-16));
#1369=DIRECTION('ref_axis',(0.,-1.38777878078145E-16,-1.));
#1370=DIRECTION('center_axis',(1.,0.,0.));
#1371=DIRECTION('ref_axis',(0.,0.,1.));
#1372=DIRECTION('center_axis',(0.,1.,0.));
#1373=DIRECTION('ref_axis',(1.,0.,0.));
#1374=DIRECTION('center_axis',(0.,-1.,0.));
#1375=DIRECTION('ref_axis',(1.,0.,0.));
#1376=DIRECTION('',(0.,0.,1.));
#1377=DIRECTION('center_axis',(1.,0.,0.));
#1378=DIRECTION('ref_axis',(0.,0.,1.));
#1379=DIRECTION('',(0.,-1.,0.));
#1380=DIRECTION('',(0.,0.,1.));
#1381=DIRECTION('',(0.,-1.,0.));
#1382=DIRECTION('center_axis',(0.,-1.,0.));
#1383=DIRECTION('ref_axis',(1.,0.,0.));
#1384=DIRECTION('center_axis',(0.,-1.,0.));
#1385=DIRECTION('ref_axis',(1.,0.,0.));
#1386=DIRECTION('',(0.,1.,0.));
#1387=DIRECTION('center_axis',(0.,-1.,0.));
#1388=DIRECTION('ref_axis',(1.,0.,0.));
#1389=DIRECTION('center_axis',(0.,1.,0.));
#1390=DIRECTION('ref_axis',(1.,0.,0.));
#1391=DIRECTION('',(0.,0.,1.));
#1392=DIRECTION('',(1.,0.,0.));
#1393=DIRECTION('',(0.,0.,1.));
#1394=DIRECTION('',(1.,0.,0.));
#1395=DIRECTION('',(0.,0.,1.));
#1396=DIRECTION('',(1.,0.,0.));
#1397=DIRECTION('',(0.,0.,1.));
#1398=DIRECTION('',(1.,0.,0.));
#1399=DIRECTION('',(0.,0.,1.));
#1400=DIRECTION('',(1.,0.,0.));
#1401=DIRECTION('',(0.,0.,1.));
#1402=DIRECTION('',(1.,0.,0.));
#1403=DIRECTION('',(0.,0.,1.));
#1404=DIRECTION('',(2.22044604925031E-16,1.,0.));
#1405=DIRECTION('',(0.,0.,1.));
#1406=DIRECTION('',(1.,0.,0.));
#1407=DIRECTION('',(0.,0.,1.));
#1408=DIRECTION('',(1.,0.,0.));
#1409=DIRECTION('',(0.,0.,1.));
#1410=DIRECTION('',(1.,0.,0.));
#1411=DIRECTION('',(0.,0.,1.));
#1412=DIRECTION('',(1.,0.,0.));
#1413=DIRECTION('',(0.,0.,1.));
#1414=DIRECTION('',(1.,0.,0.));
#1415=DIRECTION('',(0.,0.,1.));
#1416=DIRECTION('',(1.,0.,0.));
#1417=DIRECTION('',(0.,0.,1.));
#1418=DIRECTION('',(2.22044604925031E-16,1.,0.));
#1419=DIRECTION('',(0.,0.,1.));
#1420=DIRECTION('',(1.,0.,0.));
#1421=DIRECTION('',(0.,0.,1.));
#1422=DIRECTION('',(1.,0.,0.));
#1423=DIRECTION('',(0.,0.,1.));
#1424=DIRECTION('',(1.,0.,0.));
#1425=CARTESIAN_POINT('',(0.,0.,0.));
#1426=CARTESIAN_POINT('',(0.,0.,0.));
#1427=CARTESIAN_POINT('',(0.,0.,0.));
#1428=CARTESIAN_POINT('Origin',(-25.1,-1.6,0.4));
#1429=CARTESIAN_POINT('',(25.,1.6,0.4));
#1430=CARTESIAN_POINT('',(25.,-1.6,0.4));
#1431=CARTESIAN_POINT('',(25.,-1.8,0.4));
#1432=CARTESIAN_POINT('',(-25.,1.6,0.4));
#1433=CARTESIAN_POINT('',(-25.1,1.6,0.4));
#1434=CARTESIAN_POINT('',(-25.,-1.6,0.4));
#1435=CARTESIAN_POINT('',(-25.,0.2,0.4));
#1436=CARTESIAN_POINT('',(-25.1,-1.6,0.4));
#1437=CARTESIAN_POINT('Origin',(-25.1,-1.6,3.6));
#1438=CARTESIAN_POINT('',(25.,-1.6,3.6));
#1439=CARTESIAN_POINT('',(25.,-1.6,1.8));
#1440=CARTESIAN_POINT('',(-25.,-1.6,3.6));
#1441=CARTESIAN_POINT('',(-25.,-1.6,1.8));
#1442=CARTESIAN_POINT('',(-25.1,-1.6,3.6));
#1443=CARTESIAN_POINT('Origin',(-25.1,1.6,3.6));
#1444=CARTESIAN_POINT('',(25.,1.6,3.6));
#1445=CARTESIAN_POINT('',(25.,-0.2,3.6));
#1446=CARTESIAN_POINT('',(-25.,1.6,3.6));
#1447=CARTESIAN_POINT('',(-25.,1.8,3.6));
#1448=CARTESIAN_POINT('',(-25.1,1.6,3.6));
#1449=CARTESIAN_POINT('Origin',(-25.1,1.6,0.4));
#1450=CARTESIAN_POINT('',(25.,1.6,0.2));
#1451=CARTESIAN_POINT('',(-25.,1.6,0.2));
#1452=CARTESIAN_POINT('Origin',(25.,2.,0.));
#1453=CARTESIAN_POINT('',(25.,2.,0.));
#1454=CARTESIAN_POINT('',(-25.,2.,0.));
#1455=CARTESIAN_POINT('',(25.,2.,0.));
#1456=CARTESIAN_POINT('',(-25.,2.,4.));
#1457=CARTESIAN_POINT('',(-25.,2.,0.));
#1458=CARTESIAN_POINT('',(25.,2.,4.));
#1459=CARTESIAN_POINT('',(25.,2.,4.));
#1460=CARTESIAN_POINT('',(25.,2.,0.));
#1461=CARTESIAN_POINT('Origin',(25.,-2.,0.));
#1462=CARTESIAN_POINT('',(25.,-2.,0.));
#1463=CARTESIAN_POINT('',(25.,-2.,0.));
#1464=CARTESIAN_POINT('',(25.,-2.,4.));
#1465=CARTESIAN_POINT('',(25.,-2.,4.));
#1466=CARTESIAN_POINT('',(25.,-2.,0.));
#1467=CARTESIAN_POINT('Origin',(-25.,-2.,0.));
#1468=CARTESIAN_POINT('',(-25.,-2.,0.));
#1469=CARTESIAN_POINT('',(-25.,-2.,0.));
#1470=CARTESIAN_POINT('',(-25.,-2.,4.));
#1471=CARTESIAN_POINT('',(-25.,-2.,4.));
#1472=CARTESIAN_POINT('',(-25.,-2.,0.));
#1473=CARTESIAN_POINT('Origin',(-25.,2.,0.));
#1474=CARTESIAN_POINT('',(-25.,2.,0.));
#1475=CARTESIAN_POINT('',(-25.,2.,4.));
#1476=CARTESIAN_POINT('Origin',(0.,0.,4.));
#1477=CARTESIAN_POINT('Origin',(0.,0.,0.));
#1478=CARTESIAN_POINT('',(0.,0.,0.));
#1479=CARTESIAN_POINT('Origin',(-21.,-0.7,-2.));
#1480=CARTESIAN_POINT('',(-21.51,-0.6,-2.));
#1481=CARTESIAN_POINT('Origin',(-21.,-0.6,-2.));
#1482=CARTESIAN_POINT('',(-21.51,0.6,-2.));
#1483=CARTESIAN_POINT('',(-21.51,-0.7,-2.));
#1484=CARTESIAN_POINT('Origin',(-21.,0.6,-2.));
#1485=CARTESIAN_POINT('Origin',(-23.,-0.6,-2.));
#1486=CARTESIAN_POINT('',(-23.,-0.6,0.));
#1487=CARTESIAN_POINT('',(-23.,-0.6,-2.));
#1488=CARTESIAN_POINT('',(-23.,-0.6,0.));
#1489=CARTESIAN_POINT('',(-23.,0.6,0.));
#1490=CARTESIAN_POINT('',(-23.,-0.6,0.));
#1491=CARTESIAN_POINT('',(-23.,0.6,-2.));
#1492=CARTESIAN_POINT('',(-23.,0.6,0.));
#1493=CARTESIAN_POINT('',(-23.,-0.6,-2.));
#1494=CARTESIAN_POINT('Origin',(-19.,-0.6,0.));
#1495=CARTESIAN_POINT('',(-19.,-0.6,-2.));
#1496=CARTESIAN_POINT('',(-19.,-0.6,0.));
#1497=CARTESIAN_POINT('',(-19.,-0.6,-2.));
#1498=CARTESIAN_POINT('',(-19.,0.6,-2.));
#1499=CARTESIAN_POINT('',(-19.,-0.6,-2.));
#1500=CARTESIAN_POINT('',(-19.,0.6,0.));
#1501=CARTESIAN_POINT('',(-19.,0.6,-2.));
#1502=CARTESIAN_POINT('',(-19.,-0.6,0.));
#1503=CARTESIAN_POINT('Origin',(-23.,-0.6,0.));
#1504=CARTESIAN_POINT('',(-19.,0.6,0.));
#1505=CARTESIAN_POINT('',(-19.,-0.6,0.));
#1506=CARTESIAN_POINT('Origin',(-21.,0.6,-2.));
#1507=CARTESIAN_POINT('Origin',(-21.,0.6,-2.));
#1508=CARTESIAN_POINT('Origin',(-21.,-0.6,-2.));
#1509=CARTESIAN_POINT('Origin',(-21.,-0.6,-2.));
#1510=CARTESIAN_POINT('Origin',(-21.,-0.6,-2.));
#1511=CARTESIAN_POINT('',(0.,0.,0.));
#1512=CARTESIAN_POINT('',(0.,0.,0.));
#1513=CARTESIAN_POINT('',(42.,0.,0.));
#1514=CARTESIAN_POINT('',(21.,0.,4.));
#1515=CARTESIAN_POINT('',(0.,0.,0.));
#1516=CARTESIAN_POINT('',(0.,0.,0.));
#1517=CARTESIAN_POINT('',(0.,0.,0.));
#1518=CARTESIAN_POINT('Origin',(-21.,-1.9,-2.));
#1519=CARTESIAN_POINT('',(-21.515,1.,-2.));
#1520=CARTESIAN_POINT('Origin',(-21.,1.,-2.));
#1521=CARTESIAN_POINT('',(-21.515,1.8,-2.));
#1522=CARTESIAN_POINT('',(-21.515,-1.9,-2.));
#1523=CARTESIAN_POINT('Origin',(-21.,1.8,-2.));
#1524=CARTESIAN_POINT('Origin',(-21.,-1.9,-2.));
#1525=CARTESIAN_POINT('',(-21.515,-1.8,-2.));
#1526=CARTESIAN_POINT('Origin',(-21.,-1.8,-2.));
#1527=CARTESIAN_POINT('',(-21.515,-1.,-2.));
#1528=CARTESIAN_POINT('',(-21.515,-1.9,-2.));
#1529=CARTESIAN_POINT('Origin',(-21.,-1.,-2.));
#1530=CARTESIAN_POINT('Origin',(-22.,-1.8,-1.));
#1531=CARTESIAN_POINT('',(-22.,-1.8,-6.));
#1532=CARTESIAN_POINT('',(-22.,-1.8,-1.));
#1533=CARTESIAN_POINT('',(-22.,-1.8,-6.));
#1534=CARTESIAN_POINT('',(-20.,-1.8,-6.));
#1535=CARTESIAN_POINT('',(-22.,-1.8,-6.));
#1536=CARTESIAN_POINT('',(-20.,-1.8,-1.));
#1537=CARTESIAN_POINT('',(-20.,-1.8,-6.));
#1538=CARTESIAN_POINT('',(-22.,-1.8,-1.));
#1539=CARTESIAN_POINT('Origin',(-22.,-1.,-1.));
#1540=CARTESIAN_POINT('',(-22.,-1.,-1.));
#1541=CARTESIAN_POINT('',(-22.,-1.8,-1.));
#1542=CARTESIAN_POINT('',(-20.,-1.,-1.));
#1543=CARTESIAN_POINT('',(-20.,-1.8,-1.));
#1544=CARTESIAN_POINT('',(-22.,-1.,-1.));
#1545=CARTESIAN_POINT('Origin',(-22.,-1.,-5.));
#1546=CARTESIAN_POINT('',(-22.,-1.,-5.));
#1547=CARTESIAN_POINT('',(-22.,-1.,-1.));
#1548=CARTESIAN_POINT('',(-20.,-1.,-5.));
#1549=CARTESIAN_POINT('',(-20.,-1.,-1.));
#1550=CARTESIAN_POINT('',(-22.,-1.,-5.));
#1551=CARTESIAN_POINT('Origin',(-22.,1.,-5.));
#1552=CARTESIAN_POINT('',(-22.,1.,-5.));
#1553=CARTESIAN_POINT('',(-22.,-1.,-5.));
#1554=CARTESIAN_POINT('',(-20.,1.,-5.));
#1555=CARTESIAN_POINT('',(-20.,-1.,-5.));
#1556=CARTESIAN_POINT('',(-22.,1.,-5.));
#1557=CARTESIAN_POINT('Origin',(-22.,1.,-1.));
#1558=CARTESIAN_POINT('',(-22.,1.,-1.));
#1559=CARTESIAN_POINT('',(-22.,1.,-5.));
#1560=CARTESIAN_POINT('',(-20.,1.,-1.));
#1561=CARTESIAN_POINT('',(-20.,1.,-5.));
#1562=CARTESIAN_POINT('',(-22.,1.,-1.));
#1563=CARTESIAN_POINT('Origin',(-22.,1.8,-1.));
#1564=CARTESIAN_POINT('',(-22.,1.8,-1.));
#1565=CARTESIAN_POINT('',(-22.,1.,-1.));
#1566=CARTESIAN_POINT('',(-20.,1.8,-1.));
#1567=CARTESIAN_POINT('',(-20.,1.,-1.));
#1568=CARTESIAN_POINT('',(-22.,1.8,-1.));
#1569=CARTESIAN_POINT('Origin',(-22.,1.8,-6.));
#1570=CARTESIAN_POINT('',(-22.,1.8,-6.));
#1571=CARTESIAN_POINT('',(-22.,1.8,-1.));
#1572=CARTESIAN_POINT('',(-20.,1.8,-6.));
#1573=CARTESIAN_POINT('',(-20.,1.8,-1.));
#1574=CARTESIAN_POINT('',(-22.,1.8,-6.));
#1575=CARTESIAN_POINT('Origin',(-22.,-1.8,-6.));
#1576=CARTESIAN_POINT('',(-22.,1.8,-6.));
#1577=CARTESIAN_POINT('',(-20.,1.8,-6.));
#1578=CARTESIAN_POINT('Origin',(-20.,0.,-3.5));
#1579=CARTESIAN_POINT('Origin',(-22.,0.,-3.5));
#1580=CARTESIAN_POINT('',(0.,0.,0.));
#1581=CARTESIAN_POINT('Origin',(-21.,0.61,-2.));
#1582=CARTESIAN_POINT('',(-21.51,0.99,-2.));
#1583=CARTESIAN_POINT('Origin',(-21.,0.99,-2.));
#1584=CARTESIAN_POINT('',(-21.51,0.61,-2.));
#1585=CARTESIAN_POINT('',(-21.51,0.61,-2.));
#1586=CARTESIAN_POINT('Origin',(-21.,0.61,-2.));
#1587=CARTESIAN_POINT('Origin',(-21.,0.61,-2.));
#1588=CARTESIAN_POINT('',(-21.9,0.99,-2.));
#1589=CARTESIAN_POINT('Origin',(-21.,0.99,-2.));
#1590=CARTESIAN_POINT('',(-21.9,0.61,-2.));
#1591=CARTESIAN_POINT('',(-21.9,0.61,-2.));
#1592=CARTESIAN_POINT('Origin',(-21.,0.61,-2.));
#1593=CARTESIAN_POINT('Origin',(-21.,0.99,-2.));
#1594=CARTESIAN_POINT('Origin',(-21.,0.61,-2.));
#1595=CARTESIAN_POINT('',(0.,0.,0.));
#1596=CARTESIAN_POINT('Origin',(0.,-4.5,0.));
#1597=CARTESIAN_POINT('',(-0.47370877129308,-4.5,0.16));
#1598=CARTESIAN_POINT('',(-0.5,-4.66,-2.19425525987998E-17));
#1599=CARTESIAN_POINT('Ctrl Pts',(-0.47370877129308,-4.5,0.16));
#1600=CARTESIAN_POINT('Ctrl Pts',(-0.47370877129308,-4.520248682356,0.16));
#1601=CARTESIAN_POINT('Ctrl Pts',(-0.47514325949633,-4.54174042142149,0.155923994634429));
#1602=CARTESIAN_POINT('Ctrl Pts',(-0.480206450087542,-4.58111342508711,
0.13955347049286));
#1603=CARTESIAN_POINT('Ctrl Pts',(-0.483749754411139,-4.59900844138689,
0.127265728592806));
#1604=CARTESIAN_POINT('Ctrl Pts',(-0.490312616976052,-4.62726021172536,
0.0990139582543377));
#1605=CARTESIAN_POINT('Ctrl Pts',(-0.493774986141774,-4.6395522112502,0.0811167261268817));
#1606=CARTESIAN_POINT('Ctrl Pts',(-0.498649979553188,-4.65592589713458,
0.0417355732628882));
#1607=CARTESIAN_POINT('Ctrl Pts',(-0.5,-4.66,0.0202407757727682));
#1608=CARTESIAN_POINT('Ctrl Pts',(-0.5,-4.66,-2.42861286636753E-17));
#1609=CARTESIAN_POINT('',(0.47370877129308,-4.5,0.16));
#1610=CARTESIAN_POINT('',(0.,-4.5,0.16));
#1611=CARTESIAN_POINT('Ctrl Pts',(0.47370877129308,-4.5,0.16));
#1612=CARTESIAN_POINT('Ctrl Pts',(0.47370877129308,-4.479751317644,0.16));
#1613=CARTESIAN_POINT('Ctrl Pts',(0.47514325949633,-4.45825957857851,0.155923994634429));
#1614=CARTESIAN_POINT('Ctrl Pts',(0.480206450087542,-4.41888657491289,0.139553470492859));
#1615=CARTESIAN_POINT('Ctrl Pts',(0.483749754411139,-4.40099155861311,0.127265728592806));
#1616=CARTESIAN_POINT('Ctrl Pts',(0.490312616976052,-4.37273978827464,0.0990139582543375));
#1617=CARTESIAN_POINT('Ctrl Pts',(0.493774986141774,-4.3604477887498,0.0811167261268814));
#1618=CARTESIAN_POINT('Ctrl Pts',(0.498649979553188,-4.34407410286542,0.0417355732628877));
#1619=CARTESIAN_POINT('Ctrl Pts',(0.5,-4.34,0.020240775772768));
#1620=CARTESIAN_POINT('Ctrl Pts',(0.5,-4.34,-0.0202407757727682));
#1621=CARTESIAN_POINT('Ctrl Pts',(0.498649979553188,-4.34407410286542,-0.0417355732628882));
#1622=CARTESIAN_POINT('Ctrl Pts',(0.493774986141774,-4.3604477887498,-0.0811167261268817));
#1623=CARTESIAN_POINT('Ctrl Pts',(0.490312616976052,-4.37273978827464,-0.0990139582543377));
#1624=CARTESIAN_POINT('Ctrl Pts',(0.483749754411139,-4.40099155861311,-0.127265728592806));
#1625=CARTESIAN_POINT('Ctrl Pts',(0.480206450087542,-4.41888657491289,-0.13955347049286));
#1626=CARTESIAN_POINT('Ctrl Pts',(0.47514325949633,-4.45825957857851,-0.155923994634429));
#1627=CARTESIAN_POINT('Ctrl Pts',(0.47370877129308,-4.479751317644,-0.16));
#1628=CARTESIAN_POINT('Ctrl Pts',(0.47370877129308,-4.520248682356,-0.16));
#1629=CARTESIAN_POINT('Ctrl Pts',(0.47514325949633,-4.54174042142149,-0.155923994634429));
#1630=CARTESIAN_POINT('Ctrl Pts',(0.480206450087542,-4.58111342508711,-0.139553470492859));
#1631=CARTESIAN_POINT('Ctrl Pts',(0.483749754411139,-4.59900844138689,-0.127265728592806));
#1632=CARTESIAN_POINT('Ctrl Pts',(0.490312616976052,-4.62726021172536,-0.0990139582543375));
#1633=CARTESIAN_POINT('Ctrl Pts',(0.493774986141774,-4.6395522112502,-0.0811167261268813));
#1634=CARTESIAN_POINT('Ctrl Pts',(0.498649979553188,-4.65592589713458,-0.041735573262888));
#1635=CARTESIAN_POINT('Ctrl Pts',(0.5,-4.66,-0.0202407757727681));
#1636=CARTESIAN_POINT('Ctrl Pts',(0.5,-4.66,0.0202407757727682));
#1637=CARTESIAN_POINT('Ctrl Pts',(0.498649979553188,-4.65592589713458,0.0417355732628882));
#1638=CARTESIAN_POINT('Ctrl Pts',(0.493774986141774,-4.6395522112502,0.0811167261268817));
#1639=CARTESIAN_POINT('Ctrl Pts',(0.490312616976052,-4.62726021172536,0.0990139582543377));
#1640=CARTESIAN_POINT('Ctrl Pts',(0.483749754411139,-4.59900844138689,0.127265728592806));
#1641=CARTESIAN_POINT('Ctrl Pts',(0.480206450087542,-4.58111342508711,0.13955347049286));
#1642=CARTESIAN_POINT('Ctrl Pts',(0.47514325949633,-4.54174042142149,0.155923994634429));
#1643=CARTESIAN_POINT('Ctrl Pts',(0.47370877129308,-4.520248682356,0.16));
#1644=CARTESIAN_POINT('Ctrl Pts',(0.47370877129308,-4.5,0.16));
#1645=CARTESIAN_POINT('',(-0.5,-4.34,-4.01571490965563E-17));
#1646=CARTESIAN_POINT('Ctrl Pts',(-0.5,-4.34,-2.08166817117217E-17));
#1647=CARTESIAN_POINT('Ctrl Pts',(-0.5,-4.34,0.0202407757727681));
#1648=CARTESIAN_POINT('Ctrl Pts',(-0.498649979553188,-4.34407410286542,
0.041735573262888));
#1649=CARTESIAN_POINT('Ctrl Pts',(-0.493774986141774,-4.3604477887498,0.0811167261268813));
#1650=CARTESIAN_POINT('Ctrl Pts',(-0.490312616976052,-4.37273978827464,
0.0990139582543375));
#1651=CARTESIAN_POINT('Ctrl Pts',(-0.483749754411139,-4.40099155861311,
0.127265728592806));
#1652=CARTESIAN_POINT('Ctrl Pts',(-0.480206450087542,-4.41888657491289,
0.139553470492859));
#1653=CARTESIAN_POINT('Ctrl Pts',(-0.47514325949633,-4.45825957857851,0.155923994634429));
#1654=CARTESIAN_POINT('Ctrl Pts',(-0.47370877129308,-4.479751317644,0.16));
#1655=CARTESIAN_POINT('Ctrl Pts',(-0.47370877129308,-4.5,0.16));
#1656=CARTESIAN_POINT('Ctrl Pts',(-0.5,-4.66,1.38777878078145E-17));
#1657=CARTESIAN_POINT('Ctrl Pts',(-0.5,-4.66,-0.0202407757727681));
#1658=CARTESIAN_POINT('Ctrl Pts',(-0.498649979553188,-4.65592589713458,
-0.041735573262888));
#1659=CARTESIAN_POINT('Ctrl Pts',(-0.493774986141774,-4.6395522112502,-0.0811167261268813));
#1660=CARTESIAN_POINT('Ctrl Pts',(-0.490312616976052,-4.62726021172536,
-0.0990139582543375));
#1661=CARTESIAN_POINT('Ctrl Pts',(-0.483749754411139,-4.59900844138689,
-0.127265728592806));
#1662=CARTESIAN_POINT('Ctrl Pts',(-0.480206450087542,-4.58111342508711,
-0.139553470492859));
#1663=CARTESIAN_POINT('Ctrl Pts',(-0.47514325949633,-4.54174042142149,-0.155923994634429));
#1664=CARTESIAN_POINT('Ctrl Pts',(-0.47370877129308,-4.520248682356,-0.16));
#1665=CARTESIAN_POINT('Ctrl Pts',(-0.47370877129308,-4.479751317644,-0.16));
#1666=CARTESIAN_POINT('Ctrl Pts',(-0.47514325949633,-4.45825957857851,-0.155923994634429));
#1667=CARTESIAN_POINT('Ctrl Pts',(-0.480206450087542,-4.41888657491289,
-0.13955347049286));
#1668=CARTESIAN_POINT('Ctrl Pts',(-0.483749754411139,-4.40099155861311,
-0.127265728592806));
#1669=CARTESIAN_POINT('Ctrl Pts',(-0.490312616976052,-4.37273978827464,
-0.0990139582543377));
#1670=CARTESIAN_POINT('Ctrl Pts',(-0.493774986141774,-4.3604477887498,-0.0811167261268817));
#1671=CARTESIAN_POINT('Ctrl Pts',(-0.498649979553188,-4.34407410286542,
-0.0417355732628882));
#1672=CARTESIAN_POINT('Ctrl Pts',(-0.5,-4.34,-0.0202407757727682));
#1673=CARTESIAN_POINT('Ctrl Pts',(-0.5,-4.34,-1.73472347597681E-17));
#1674=CARTESIAN_POINT('Origin',(0.85,0.4,0.));
#1675=CARTESIAN_POINT('',(-0.85,0.4,-1.04094977927525E-16));
#1676=CARTESIAN_POINT('Origin',(0.,0.4,0.));
#1677=CARTESIAN_POINT('Origin',(0.,0.375,0.));
#1678=CARTESIAN_POINT('',(-0.9,0.35,-1.10218211923262E-16));
#1679=CARTESIAN_POINT('Origin',(0.,0.35,0.));
#1680=CARTESIAN_POINT('',(-0.875,0.375,-1.07156594925393E-16));
#1681=CARTESIAN_POINT('Origin',(0.,0.175,0.));
#1682=CARTESIAN_POINT('',(-0.9,0.,-1.10218211923262E-16));
#1683=CARTESIAN_POINT('Origin',(0.,0.,0.));
#1684=CARTESIAN_POINT('',(-0.9,0.175,-1.10218211923262E-16));
#1685=CARTESIAN_POINT('Origin',(0.5,0.,0.));
#1686=CARTESIAN_POINT('',(-0.5,0.,-6.12323399573677E-17));
#1687=CARTESIAN_POINT('Origin',(0.,0.,0.));
#1688=CARTESIAN_POINT('Origin',(0.,-2.435,0.));
#1689=CARTESIAN_POINT('',(-0.5,-4.87,-6.12323399573677E-17));
#1690=CARTESIAN_POINT('Origin',(0.,-4.87,0.));
#1691=CARTESIAN_POINT('',(-0.5,-2.435,-6.12323399573677E-17));
#1692=CARTESIAN_POINT('',(-0.5,-2.435,-6.12323399573677E-17));
#1693=CARTESIAN_POINT('Origin',(0.,-4.935,0.));
#1694=CARTESIAN_POINT('',(-0.37,-5.,-4.53119315684521E-17));
#1695=CARTESIAN_POINT('Origin',(0.,-5.,0.));
#1696=CARTESIAN_POINT('',(-0.435,-4.935,-5.32721357629099E-17));
#1697=CARTESIAN_POINT('Origin',(0.,-5.,0.));
#1698=CARTESIAN_POINT('',(0.,0.,0.));
#1699=CARTESIAN_POINT('Origin',(0.,0.,0.));
#1700=CARTESIAN_POINT('',(-0.525,0.2,6.4293956955236E-17));
#1701=CARTESIAN_POINT('Origin',(0.,0.2,0.));
#1702=CARTESIAN_POINT('',(-0.525,0.,6.4293956955236E-17));
#1703=CARTESIAN_POINT('',(-0.525,0.,6.4293956955236E-17));
#1704=CARTESIAN_POINT('Origin',(0.,0.,0.));
#1705=CARTESIAN_POINT('Origin',(0.,0.,0.));
#1706=CARTESIAN_POINT('',(-1.,0.2,1.22464679914735E-16));
#1707=CARTESIAN_POINT('Origin',(0.,0.2,0.));
#1708=CARTESIAN_POINT('',(-1.,0.,1.22464679914735E-16));
#1709=CARTESIAN_POINT('',(-1.,0.,1.22464679914735E-16));
#1710=CARTESIAN_POINT('Origin',(0.,0.,0.));
#1711=CARTESIAN_POINT('Origin',(0.,0.2,0.));
#1712=CARTESIAN_POINT('Origin',(0.,0.,0.));
#1713=CARTESIAN_POINT('',(0.,0.,0.));
#1714=CARTESIAN_POINT('Origin',(0.,0.24,0.));
#1715=CARTESIAN_POINT('',(-1.95943487863577E-17,0.24,-0.08));
#1716=CARTESIAN_POINT('Origin',(0.,0.24,-0.24));
#1717=CARTESIAN_POINT('Origin',(1.95943487863577E-17,0.24,0.));
#1718=CARTESIAN_POINT('',(0.16,-9.79717439317883E-18,1.46957615897682E-17));
#1719=CARTESIAN_POINT('',(-0.16,-9.79717439317883E-18,1.46957615897682E-17));
#1720=CARTESIAN_POINT('Ctrl Pts',(0.16,-9.79717439317883E-18,1.46957615897682E-17));
#1721=CARTESIAN_POINT('Ctrl Pts',(0.16,-0.000181822110339334,0.000181822110339339));
#1722=CARTESIAN_POINT('Ctrl Pts',(0.159999690069269,-0.000363540844324622,
0.000363747464878571));
#1723=CARTESIAN_POINT('Ctrl Pts',(0.159953479738417,-0.0138798266221246,
0.0139107352627986));
#1724=CARTESIAN_POINT('Ctrl Pts',(0.158232443771481,-0.0266233430820533,
0.0277973751356497));
#1725=CARTESIAN_POINT('Ctrl Pts',(0.149940017697612,-0.0530153061725048,
0.058442405232979));
#1726=CARTESIAN_POINT('Ctrl Pts',(0.142540414573103,-0.0662634124922917,
0.0751206840235135));
#1727=CARTESIAN_POINT('Ctrl Pts',(0.122571789881533,-0.0881367971480854,
0.104109120837503));
#1728=CARTESIAN_POINT('Ctrl Pts',(0.111018055346349,-0.0970398395589147,
0.116543563059122));
#1729=CARTESIAN_POINT('Ctrl Pts',(0.0824796164288417,-0.112218107746775,
0.138327679583944));
#1730=CARTESIAN_POINT('Ctrl Pts',(0.0655757961780097,-0.118179284966592,
0.147245809917584));
#1731=CARTESIAN_POINT('Ctrl Pts',(0.0318466054620204,-0.125035966654145,
0.157587272150341));
#1732=CARTESIAN_POINT('Ctrl Pts',(0.0160332282918615,-0.126606055596467,
0.16));
#1733=CARTESIAN_POINT('Ctrl Pts',(-0.0160332282918615,-0.126606055596467,
0.16));
#1734=CARTESIAN_POINT('Ctrl Pts',(-0.0318466054620203,-0.125035966654145,
0.157587272150341));
#1735=CARTESIAN_POINT('Ctrl Pts',(-0.0655757961780098,-0.118179284966592,
0.147245809917584));
#1736=CARTESIAN_POINT('Ctrl Pts',(-0.0824796164288418,-0.112218107746775,
0.138327679583943));
#1737=CARTESIAN_POINT('Ctrl Pts',(-0.111018055346349,-0.0970398395589147,
0.116543563059122));
#1738=CARTESIAN_POINT('Ctrl Pts',(-0.122571789881533,-0.0881367971480853,
0.104109120837503));
#1739=CARTESIAN_POINT('Ctrl Pts',(-0.142540414573103,-0.0662634124922916,
0.0751206840235135));
#1740=CARTESIAN_POINT('Ctrl Pts',(-0.149940017697612,-0.0530153061725049,
0.0584424052329791));
#1741=CARTESIAN_POINT('Ctrl Pts',(-0.158232443771481,-0.0266233430820551,
0.0277973751356518));
#1742=CARTESIAN_POINT('Ctrl Pts',(-0.159953479738417,-0.0138798266221373,
0.0139107352628116));
#1743=CARTESIAN_POINT('Ctrl Pts',(-0.159999690069269,-0.000363540844323022,
0.000363747464876927));
#1744=CARTESIAN_POINT('Ctrl Pts',(-0.16,-0.000181822110340974,0.000181822110340979));
#1745=CARTESIAN_POINT('Ctrl Pts',(-0.16,-9.79717439317883E-18,1.46957615897682E-17));
#1746=CARTESIAN_POINT('Ctrl Pts',(-0.16,-9.79717439317883E-18,1.46957615897682E-17));
#1747=CARTESIAN_POINT('Ctrl Pts',(-0.16,-0.000181822110343777,-0.000181822110343752));
#1748=CARTESIAN_POINT('Ctrl Pts',(-0.159999690069269,-0.000363540844320234,
-0.000363747464874079));
#1749=CARTESIAN_POINT('Ctrl Pts',(-0.159953479738416,-0.013879826622296,
-0.0139107352629724));
#1750=CARTESIAN_POINT('Ctrl Pts',(-0.158232443771474,-0.0266233430820775,
-0.0277973751356779));
#1751=CARTESIAN_POINT('Ctrl Pts',(-0.149940017697612,-0.053015306172505,
-0.0584424052329793));
#1752=CARTESIAN_POINT('Ctrl Pts',(-0.142540414573103,-0.0662634124922918,
-0.0751206840235137));
#1753=CARTESIAN_POINT('Ctrl Pts',(-0.122571789881533,-0.0881367971480854,
-0.104109120837503));
#1754=CARTESIAN_POINT('Ctrl Pts',(-0.111018055346349,-0.0970398395589147,
-0.116543563059122));
#1755=CARTESIAN_POINT('Ctrl Pts',(-0.0824796164288418,-0.112218107746775,
-0.138327679583943));
#1756=CARTESIAN_POINT('Ctrl Pts',(-0.0655757961780097,-0.118179284966592,
-0.147245809917584));
#1757=CARTESIAN_POINT('Ctrl Pts',(-0.0318466054620201,-0.125035966654145,
-0.157587272150341));
#1758=CARTESIAN_POINT('Ctrl Pts',(-0.0160332282918614,-0.126606055596467,
-0.16));
#1759=CARTESIAN_POINT('Ctrl Pts',(0.0160332282918614,-0.126606055596467,
-0.16));
#1760=CARTESIAN_POINT('Ctrl Pts',(0.0318466054620202,-0.125035966654145,
-0.157587272150341));
#1761=CARTESIAN_POINT('Ctrl Pts',(0.0655757961780098,-0.118179284966592,
-0.147245809917584));
#1762=CARTESIAN_POINT('Ctrl Pts',(0.0824796164288418,-0.112218107746775,
-0.138327679583943));
#1763=CARTESIAN_POINT('Ctrl Pts',(0.111018055346349,-0.0970398395589148,
-0.116543563059122));
#1764=CARTESIAN_POINT('Ctrl Pts',(0.122571789881533,-0.0881367971480855,
-0.104109120837504));
#1765=CARTESIAN_POINT('Ctrl Pts',(0.142540414573103,-0.0662634124922916,
-0.0751206840235135));
#1766=CARTESIAN_POINT('Ctrl Pts',(0.149940017697612,-0.0530153061725047,
-0.058442405232979));
#1767=CARTESIAN_POINT('Ctrl Pts',(0.158232443771478,-0.0266233430820626,
-0.0277973751356607));
#1768=CARTESIAN_POINT('Ctrl Pts',(0.159953479738417,-0.0138798266221904,
-0.0139107352628652));
#1769=CARTESIAN_POINT('Ctrl Pts',(0.159999690069269,-0.000363540844323479,
-0.000363747464877385));
#1770=CARTESIAN_POINT('Ctrl Pts',(0.16,-0.000181822110340484,-0.00018182211034046));
#1771=CARTESIAN_POINT('Ctrl Pts',(0.16,-9.79717439317883E-18,1.46957615897682E-17));
#1772=CARTESIAN_POINT('Origin',(0.08,-2.02,0.));
#1773=CARTESIAN_POINT('',(0.,-2.02,-0.16));
#1774=CARTESIAN_POINT('',(0.,-2.02,0.16));
#1775=CARTESIAN_POINT('Origin',(0.,-2.02,0.));
#1776=CARTESIAN_POINT('',(0.,-2.02,-0.08));
#1777=CARTESIAN_POINT('Origin',(0.,0.,-0.16));
#1778=CARTESIAN_POINT('',(0.,-2.5,0.16));
#1779=CARTESIAN_POINT('',(0.,0.,0.16));
#1780=CARTESIAN_POINT('',(0.,-2.5,-0.16));
#1781=CARTESIAN_POINT('',(0.,-2.5,-0.17));
#1782=CARTESIAN_POINT('',(0.,0.,-0.16));
#1783=CARTESIAN_POINT('Origin',(0.,0.,0.));
#1784=CARTESIAN_POINT('',(-0.16,-2.5,-1.95943487863577E-17));
#1785=CARTESIAN_POINT('Origin',(0.,-2.5,0.));
#1786=CARTESIAN_POINT('',(-0.16,0.,-1.95943487863577E-17));
#1787=CARTESIAN_POINT('Origin',(0.,-2.5,0.));
#1788=CARTESIAN_POINT('Origin',(-0.08,-2.5,0.));
#1789=CARTESIAN_POINT('',(0.,0.,0.));
#1790=CARTESIAN_POINT('',(0.,0.,0.));
#1791=CARTESIAN_POINT('',(0.,-1.6,0.));
#1792=CARTESIAN_POINT('',(-21.,2.,-2.));
#1793=CARTESIAN_POINT('',(-21.,-2.,-2.));
#1794=CARTESIAN_POINT('',(-21.,1.8,-2.));
#1795=CARTESIAN_POINT('',(-21.6,-2.5,-2.));
#1796=CARTESIAN_POINT('',(42.,0.,0.));
#1797=CARTESIAN_POINT('',(42.,0.,0.));
#1798=CARTESIAN_POINT('',(42.,-1.6,0.));
#1799=CARTESIAN_POINT('',(21.,2.,-2.));
#1800=CARTESIAN_POINT('',(21.,-2.,-2.));
#1801=CARTESIAN_POINT('',(21.,1.8,-2.));
#1802=CARTESIAN_POINT('',(20.4,-2.5,-2.));
#1803=CARTESIAN_POINT('',(0.,0.,0.));
#1804=CARTESIAN_POINT('',(0.,0.,0.));
#1805=CARTESIAN_POINT('',(0.,0.,0.));
#1806=UNCERTAINTY_MEASURE_WITH_UNIT(LENGTH_MEASURE(0.001),#1830,
'DISTANCE_ACCURACY_VALUE',
'Maximum model space distance between geometric entities at asserted c
onnectivities');
#1807=UNCERTAINTY_MEASURE_WITH_UNIT(LENGTH_MEASURE(0.001),#1830,
'DISTANCE_ACCURACY_VALUE',
'Maximum model space distance between geometric entities at asserted c
onnectivities');
#1808=UNCERTAINTY_MEASURE_WITH_UNIT(LENGTH_MEASURE(0.001),#1830,
'DISTANCE_ACCURACY_VALUE',
'Maximum model space distance between geometric entities at asserted c
onnectivities');
#1809=UNCERTAINTY_MEASURE_WITH_UNIT(LENGTH_MEASURE(0.001),#1830,
'DISTANCE_ACCURACY_VALUE',
'Maximum model space distance between geometric entities at asserted c
onnectivities');
#1810=UNCERTAINTY_MEASURE_WITH_UNIT(LENGTH_MEASURE(0.001),#1830,
'DISTANCE_ACCURACY_VALUE',
'Maximum model space distance between geometric entities at asserted c
onnectivities');
#1811=UNCERTAINTY_MEASURE_WITH_UNIT(LENGTH_MEASURE(0.001),#1830,
'DISTANCE_ACCURACY_VALUE',
'Maximum model space distance between geometric entities at asserted c
onnectivities');
#1812=UNCERTAINTY_MEASURE_WITH_UNIT(LENGTH_MEASURE(0.001),#1830,
'DISTANCE_ACCURACY_VALUE',
'Maximum model space distance between geometric entities at asserted c
onnectivities');
#1813=UNCERTAINTY_MEASURE_WITH_UNIT(LENGTH_MEASURE(0.001),#1830,
'DISTANCE_ACCURACY_VALUE',
'Maximum model space distance between geometric entities at asserted c
onnectivities');
#1814=UNCERTAINTY_MEASURE_WITH_UNIT(LENGTH_MEASURE(0.001),#1830,
'DISTANCE_ACCURACY_VALUE',
'Maximum model space distance between geometric entities at asserted c
onnectivities');
#1815=UNCERTAINTY_MEASURE_WITH_UNIT(LENGTH_MEASURE(0.001),#1830,
'DISTANCE_ACCURACY_VALUE',
'Maximum model space distance between geometric entities at asserted c
onnectivities');
#1816=UNCERTAINTY_MEASURE_WITH_UNIT(LENGTH_MEASURE(0.001),#1830,
'DISTANCE_ACCURACY_VALUE',
'Maximum model space distance between geometric entities at asserted c
onnectivities');
#1817=UNCERTAINTY_MEASURE_WITH_UNIT(LENGTH_MEASURE(0.001),#1830,
'DISTANCE_ACCURACY_VALUE',
'Maximum model space distance between geometric entities at asserted c
onnectivities');
#1818=(
GEOMETRIC_REPRESENTATION_CONTEXT(3)
GLOBAL_UNCERTAINTY_ASSIGNED_CONTEXT((#1806))
GLOBAL_UNIT_ASSIGNED_CONTEXT((#1830,#1832,#1833))
REPRESENTATION_CONTEXT('','3D')
);
#1819=(
GEOMETRIC_REPRESENTATION_CONTEXT(3)
GLOBAL_UNCERTAINTY_ASSIGNED_CONTEXT((#1807))
GLOBAL_UNIT_ASSIGNED_CONTEXT((#1830,#1832,#1833))
REPRESENTATION_CONTEXT('','3D')
);
#1820=(
GEOMETRIC_REPRESENTATION_CONTEXT(3)
GLOBAL_UNCERTAINTY_ASSIGNED_CONTEXT((#1808))
GLOBAL_UNIT_ASSIGNED_CONTEXT((#1830,#1832,#1833))
REPRESENTATION_CONTEXT('','3D')
);
#1821=(
GEOMETRIC_REPRESENTATION_CONTEXT(3)
GLOBAL_UNCERTAINTY_ASSIGNED_CONTEXT((#1809))
GLOBAL_UNIT_ASSIGNED_CONTEXT((#1830,#1832,#1833))
REPRESENTATION_CONTEXT('','3D')
);
#1822=(
GEOMETRIC_REPRESENTATION_CONTEXT(3)
GLOBAL_UNCERTAINTY_ASSIGNED_CONTEXT((#1810))
GLOBAL_UNIT_ASSIGNED_CONTEXT((#1830,#1832,#1833))
REPRESENTATION_CONTEXT('','3D')
);
#1823=(
GEOMETRIC_REPRESENTATION_CONTEXT(3)
GLOBAL_UNCERTAINTY_ASSIGNED_CONTEXT((#1811))
GLOBAL_UNIT_ASSIGNED_CONTEXT((#1830,#1832,#1833))
REPRESENTATION_CONTEXT('','3D')
);
#1824=(
GEOMETRIC_REPRESENTATION_CONTEXT(3)
GLOBAL_UNCERTAINTY_ASSIGNED_CONTEXT((#1812))
GLOBAL_UNIT_ASSIGNED_CONTEXT((#1830,#1832,#1833))
REPRESENTATION_CONTEXT('','3D')
);
#1825=(
GEOMETRIC_REPRESENTATION_CONTEXT(3)
GLOBAL_UNCERTAINTY_ASSIGNED_CONTEXT((#1813))
GLOBAL_UNIT_ASSIGNED_CONTEXT((#1830,#1832,#1833))
REPRESENTATION_CONTEXT('','3D')
);
#1826=(
GEOMETRIC_REPRESENTATION_CONTEXT(3)
GLOBAL_UNCERTAINTY_ASSIGNED_CONTEXT((#1814))
GLOBAL_UNIT_ASSIGNED_CONTEXT((#1830,#1832,#1833))
REPRESENTATION_CONTEXT('','3D')
);
#1827=(
GEOMETRIC_REPRESENTATION_CONTEXT(3)
GLOBAL_UNCERTAINTY_ASSIGNED_CONTEXT((#1815))
GLOBAL_UNIT_ASSIGNED_CONTEXT((#1830,#1832,#1833))
REPRESENTATION_CONTEXT('','3D')
);
#1828=(
GEOMETRIC_REPRESENTATION_CONTEXT(3)
GLOBAL_UNCERTAINTY_ASSIGNED_CONTEXT((#1816))
GLOBAL_UNIT_ASSIGNED_CONTEXT((#1830,#1832,#1833))
REPRESENTATION_CONTEXT('','3D')
);
#1829=(
GEOMETRIC_REPRESENTATION_CONTEXT(3)
GLOBAL_UNCERTAINTY_ASSIGNED_CONTEXT((#1817))
GLOBAL_UNIT_ASSIGNED_CONTEXT((#1830,#1832,#1833))
REPRESENTATION_CONTEXT('','3D')
);
#1830=(
LENGTH_UNIT()
NAMED_UNIT(*)
SI_UNIT(.CENTI.,.METRE.)
);
#1831=(
LENGTH_UNIT()
NAMED_UNIT(*)
SI_UNIT($,.METRE.)
);
#1832=(
NAMED_UNIT(*)
PLANE_ANGLE_UNIT()
SI_UNIT($,.RADIAN.)
);
#1833=(
NAMED_UNIT(*)
SI_UNIT($,.STERADIAN.)
SOLID_ANGLE_UNIT()
);
#1834=SHAPE_DEFINITION_REPRESENTATION(#1845,#1877);
#1835=SHAPE_DEFINITION_REPRESENTATION(#1846,#1878);
#1836=SHAPE_DEFINITION_REPRESENTATION(#1847,#1879);
#1837=SHAPE_DEFINITION_REPRESENTATION(#1848,#1880);
#1838=SHAPE_DEFINITION_REPRESENTATION(#1853,#1881);
#1839=SHAPE_DEFINITION_REPRESENTATION(#1854,#1882);
#1840=SHAPE_DEFINITION_REPRESENTATION(#1855,#1883);
#1841=SHAPE_DEFINITION_REPRESENTATION(#1856,#1884);
#1842=SHAPE_DEFINITION_REPRESENTATION(#1857,#1885);
#1843=SHAPE_DEFINITION_REPRESENTATION(#1858,#1886);
#1844=SHAPE_DEFINITION_REPRESENTATION(#1859,#1887);
#1845=PRODUCT_DEFINITION_SHAPE('',$,#1889);
#1846=PRODUCT_DEFINITION_SHAPE('',$,#1890);
#1847=PRODUCT_DEFINITION_SHAPE('',$,#1891);
#1848=PRODUCT_DEFINITION_SHAPE('',$,#1892);
#1849=PRODUCT_DEFINITION_SHAPE($,$,#83);
#1850=PRODUCT_DEFINITION_SHAPE($,$,#84);
#1851=PRODUCT_DEFINITION_SHAPE($,$,#85);
#1852=PRODUCT_DEFINITION_SHAPE($,$,#86);
#1853=PRODUCT_DEFINITION_SHAPE('',$,#1893);
#1854=PRODUCT_DEFINITION_SHAPE('',$,#1894);
#1855=PRODUCT_DEFINITION_SHAPE('',$,#1895);
#1856=PRODUCT_DEFINITION_SHAPE('',$,#1896);
#1857=PRODUCT_DEFINITION_SHAPE('',$,#1897);
#1858=PRODUCT_DEFINITION_SHAPE('',$,#1898);
#1859=PRODUCT_DEFINITION_SHAPE('',$,#1899);
#1860=PRODUCT_DEFINITION_SHAPE($,$,#87);
#1861=PRODUCT_DEFINITION_SHAPE($,$,#88);
#1862=PRODUCT_DEFINITION_SHAPE($,$,#89);
#1863=PRODUCT_DEFINITION_SHAPE($,$,#90);
#1864=PRODUCT_DEFINITION_SHAPE($,$,#91);
#1865=PRODUCT_DEFINITION_SHAPE($,$,#92);
#1866=PRODUCT_DEFINITION_SHAPE($,$,#93);
#1867=PRODUCT_DEFINITION_SHAPE($,$,#94);
#1868=PRODUCT_DEFINITION_SHAPE($,$,#95);
#1869=PRODUCT_DEFINITION_SHAPE($,$,#96);
#1870=PRODUCT_DEFINITION_SHAPE($,$,#97);
#1871=PRODUCT_DEFINITION_SHAPE($,$,#98);
#1872=PRODUCT_DEFINITION_SHAPE($,$,#99);
#1873=PRODUCT_DEFINITION_SHAPE($,$,#100);
#1874=PRODUCT_DEFINITION_SHAPE($,$,#101);
#1875=PRODUCT_DEFINITION_SHAPE($,$,#102);
#1876=PRODUCT_DEFINITION_SHAPE($,$,#103);
#1877=SHAPE_REPRESENTATION('',(#1022,#1128,#1129,#1130),#1818);
#1878=SHAPE_REPRESENTATION('',(#1023,#1047,#1048,#1049,#1050),#1819);
#1879=SHAPE_REPRESENTATION('',(#1024),#1820);
#1880=SHAPE_REPRESENTATION('',(#1035),#1821);
#1881=SHAPE_REPRESENTATION('',(#1051,#1114,#1115,#1116,#1117,#1118,#1119,
#1120),#1822);
#1882=SHAPE_REPRESENTATION('',(#1052,#1121,#1122,#1123,#1124,#1125,#1126,
#1127),#1823);
#1883=SHAPE_REPRESENTATION('',(#1053),#1824);
#1884=SHAPE_REPRESENTATION('',(#1070),#1825);
#1885=SHAPE_REPRESENTATION('',(#1079),#1826);
#1886=SHAPE_REPRESENTATION('',(#1094),#1827);
#1887=SHAPE_REPRESENTATION('',(#1103),#1828);
#1888=PRODUCT_DEFINITION_CONTEXT('part definition',#1923,'design');
#1889=PRODUCT_DEFINITION('PAT-109','PAT-109',#1900,
#1888);
#1890=PRODUCT_DEFINITION('Hollow beam and welded eyes',
'Hollow beam and welded eyes',#1901,#1888);
#1891=PRODUCT_DEFINITION('Hollow spreader beam','Hollow spreader beam',
#1902,#1888);
#1892=PRODUCT_DEFINITION('Welded eye plate','Welded eye plate',#1903,#1888);
#1893=PRODUCT_DEFINITION('Left pinned shackle','Left pinned shackle',#1904,
#1888);
#1894=PRODUCT_DEFINITION('Right pinned shackle','Right pinned shackle',
#1905,#1888);
#1895=PRODUCT_DEFINITION('Machined U shackle','Machined U shackle',#1906,
#1888);
#1896=PRODUCT_DEFINITION('Pin side spacer','Pin side spacer',#1907,#1888);
#1897=PRODUCT_DEFINITION('Clevis Pin - 10x50','Clevis Pin - 10x50',#1908,
#1888);
#1898=PRODUCT_DEFINITION('Flat Washer - M10','Flat Washer - M10',#1909,
#1888);
#1899=PRODUCT_DEFINITION('Split Pin - 3.2x25','Split Pin - 3.2x25',#1910,
#1888);
#1900=PRODUCT_DEFINITION_FORMATION('',$,#1925);
#1901=PRODUCT_DEFINITION_FORMATION('',$,#1926);
#1902=PRODUCT_DEFINITION_FORMATION('',$,#1927);
#1903=PRODUCT_DEFINITION_FORMATION('',$,#1928);
#1904=PRODUCT_DEFINITION_FORMATION('',$,#1929);
#1905=PRODUCT_DEFINITION_FORMATION('',$,#1930);
#1906=PRODUCT_DEFINITION_FORMATION('',$,#1931);
#1907=PRODUCT_DEFINITION_FORMATION('',$,#1932);
#1908=PRODUCT_DEFINITION_FORMATION('',$,#1933);
#1909=PRODUCT_DEFINITION_FORMATION('',$,#1934);
#1910=PRODUCT_DEFINITION_FORMATION('',$,#1935);
#1911=PRODUCT_RELATED_PRODUCT_CATEGORY('PAT-109','PAT-109',(#1925));
#1912=PRODUCT_RELATED_PRODUCT_CATEGORY('Hollow beam and welded eyes',
'Hollow beam and welded eyes',(#1926));
#1913=PRODUCT_RELATED_PRODUCT_CATEGORY('Hollow spreader beam',
'Hollow spreader beam',(#1927));
#1914=PRODUCT_RELATED_PRODUCT_CATEGORY('Welded eye plate',
'Welded eye plate',(#1928));
#1915=PRODUCT_RELATED_PRODUCT_CATEGORY('Left pinned shackle',
'Left pinned shackle',(#1929));
#1916=PRODUCT_RELATED_PRODUCT_CATEGORY('Right pinned shackle',
'Right pinned shackle',(#1930));
#1917=PRODUCT_RELATED_PRODUCT_CATEGORY('Machined U shackle',
'Machined U shackle',(#1931));
#1918=PRODUCT_RELATED_PRODUCT_CATEGORY('Pin side spacer',
'Pin side spacer',(#1932));
#1919=PRODUCT_RELATED_PRODUCT_CATEGORY('Clevis Pin - 10x50',
'Clevis Pin - 10x50',(#1933));
#1920=PRODUCT_RELATED_PRODUCT_CATEGORY('Flat Washer - M10',
'Flat Washer - M10',(#1934));
#1921=PRODUCT_RELATED_PRODUCT_CATEGORY('Split Pin - 3.2x25',
'Split Pin - 3.2x25',(#1935));
#1922=APPLICATION_PROTOCOL_DEFINITION('international standard',
'automotive_design',2009,#1923);
#1923=APPLICATION_CONTEXT(
'Core Data for Automotive Mechanical Design Process');
#1924=PRODUCT_CONTEXT('part definition',#1923,'mechanical');
#1925=PRODUCT('PAT-109','PAT-109',
'PAT-109',(#1924));
#1926=PRODUCT('Hollow beam and welded eyes',
'Hollow beam and welded eyes','Hollow beam and welded eyes',(#1924));
#1927=PRODUCT('Hollow spreader beam','Hollow spreader beam',
'Hollow spreader beam',(#1924));
#1928=PRODUCT('Welded eye plate','Welded eye plate','Welded eye plate',
(#1924));
#1929=PRODUCT('Left pinned shackle','Left pinned shackle',
'Left pinned shackle',(#1924));
#1930=PRODUCT('Right pinned shackle','Right pinned shackle',
'Right pinned shackle',(#1924));
#1931=PRODUCT('Machined U shackle','Machined U shackle',
'Machined U shackle',(#1924));
#1932=PRODUCT('Pin side spacer','Pin side spacer','Pin side spacer',(#1924));
#1933=PRODUCT('Clevis Pin - 10x50','Clevis Pin - 10x50',
'Clevis Pin - 10x50',(#1924));
#1934=PRODUCT('Flat Washer - M10','Flat Washer - M10',
'Flat Washer - M10',(#1924));
#1935=PRODUCT('Split Pin - 3.2x25','Split Pin - 3.2x25',
'Split Pin - 3.2x25',(#1924));
#1936=PRESENTATION_STYLE_ASSIGNMENT((#1939));
#1937=PRESENTATION_STYLE_ASSIGNMENT((#1940));
#1938=PRESENTATION_STYLE_ASSIGNMENT((#1941));
#1939=SURFACE_STYLE_USAGE(.BOTH.,#1942);
#1940=SURFACE_STYLE_USAGE(.BOTH.,#1943);
#1941=SURFACE_STYLE_USAGE(.BOTH.,#1944);
#1942=SURFACE_SIDE_STYLE('',(#1945));
#1943=SURFACE_SIDE_STYLE('',(#1946));
#1944=SURFACE_SIDE_STYLE('',(#1947));
#1945=SURFACE_STYLE_FILL_AREA(#1948);
#1946=SURFACE_STYLE_FILL_AREA(#1949);
#1947=SURFACE_STYLE_FILL_AREA(#1950);
#1948=FILL_AREA_STYLE('Steel - Satin',(#1951));
#1949=FILL_AREA_STYLE('CAD Library Painted - Engineering blue',(#1952));
#1950=FILL_AREA_STYLE('CAD Library Painted - Steel gray',(#1953));
#1951=FILL_AREA_STYLE_COLOUR('Steel - Satin',#1954);
#1952=FILL_AREA_STYLE_COLOUR('CAD Library Painted - Engineering blue',#1955);
#1953=FILL_AREA_STYLE_COLOUR('CAD Library Painted - Steel gray',#1956);
#1954=COLOUR_RGB('Steel - Satin',0.627450980392157,0.627450980392157,0.627450980392157);
#1955=COLOUR_RGB('CAD Library Painted - Engineering blue',0.12156862745098,
0.356862745098039,0.6);
#1956=COLOUR_RGB('CAD Library Painted - Steel gray',0.592156862745098,0.631372549019608,
0.67843137254902);
#1957=COLOUR_RGB('Dark Blue',0.08,0.2,0.34);
#1958=FILL_AREA_STYLE_COLOUR('',#1957);
#1959=FILL_AREA_STYLE('',(#1958));
#1960=SURFACE_STYLE_FILL_AREA(#1959);
#1961=SURFACE_SIDE_STYLE('',(#1960));
#1962=SURFACE_STYLE_USAGE(.BOTH.,#1961);
#1963=PRESENTATION_STYLE_ASSIGNMENT((#1962));
#1964=COLOUR_RGB('Light Blue',0.38,0.62,0.78);
#1965=FILL_AREA_STYLE_COLOUR('',#1964);
#1966=FILL_AREA_STYLE('',(#1965));
#1967=SURFACE_STYLE_FILL_AREA(#1966);
#1968=SURFACE_SIDE_STYLE('',(#1967));
#1969=SURFACE_STYLE_USAGE(.BOTH.,#1968);
#1970=PRESENTATION_STYLE_ASSIGNMENT((#1969));
#1971=COLOUR_RGB('Sky Blue',0.24,0.69,0.87);
#1972=FILL_AREA_STYLE_COLOUR('',#1971);
#1973=FILL_AREA_STYLE('',(#1972));
#1974=SURFACE_STYLE_FILL_AREA(#1973);
#1975=SURFACE_SIDE_STYLE('',(#1974));
#1976=SURFACE_STYLE_USAGE(.BOTH.,#1975);
#1977=PRESENTATION_STYLE_ASSIGNMENT((#1976));
#1978=COLOUR_RGB('Grey',0.48,0.52,0.57);
#1979=FILL_AREA_STYLE_COLOUR('',#1978);
#1980=FILL_AREA_STYLE('',(#1979));
#1981=SURFACE_STYLE_FILL_AREA(#1980);
#1982=SURFACE_SIDE_STYLE('',(#1981));
#1983=SURFACE_STYLE_USAGE(.BOTH.,#1982);
#1984=PRESENTATION_STYLE_ASSIGNMENT((#1983));
#1985=COLOUR_RGB('Black',0.12,0.14,0.17);
#1986=FILL_AREA_STYLE_COLOUR('',#1985);
#1987=FILL_AREA_STYLE('',(#1986));
#1988=SURFACE_STYLE_FILL_AREA(#1987);
#1989=SURFACE_SIDE_STYLE('',(#1988));
#1990=SURFACE_STYLE_USAGE(.BOTH.,#1989);
#1991=PRESENTATION_STYLE_ASSIGNMENT((#1990));
#1992=COLOUR_RGB('Off White',0.89,0.88,0.83);
#1993=FILL_AREA_STYLE_COLOUR('',#1992);
#1994=FILL_AREA_STYLE('',(#1993));
#1995=SURFACE_STYLE_FILL_AREA(#1994);
#1996=SURFACE_SIDE_STYLE('',(#1995));
#1997=SURFACE_STYLE_USAGE(.BOTH.,#1996);
#1998=PRESENTATION_STYLE_ASSIGNMENT((#1997));
ENDSEC;
END-ISO-10303-21;
